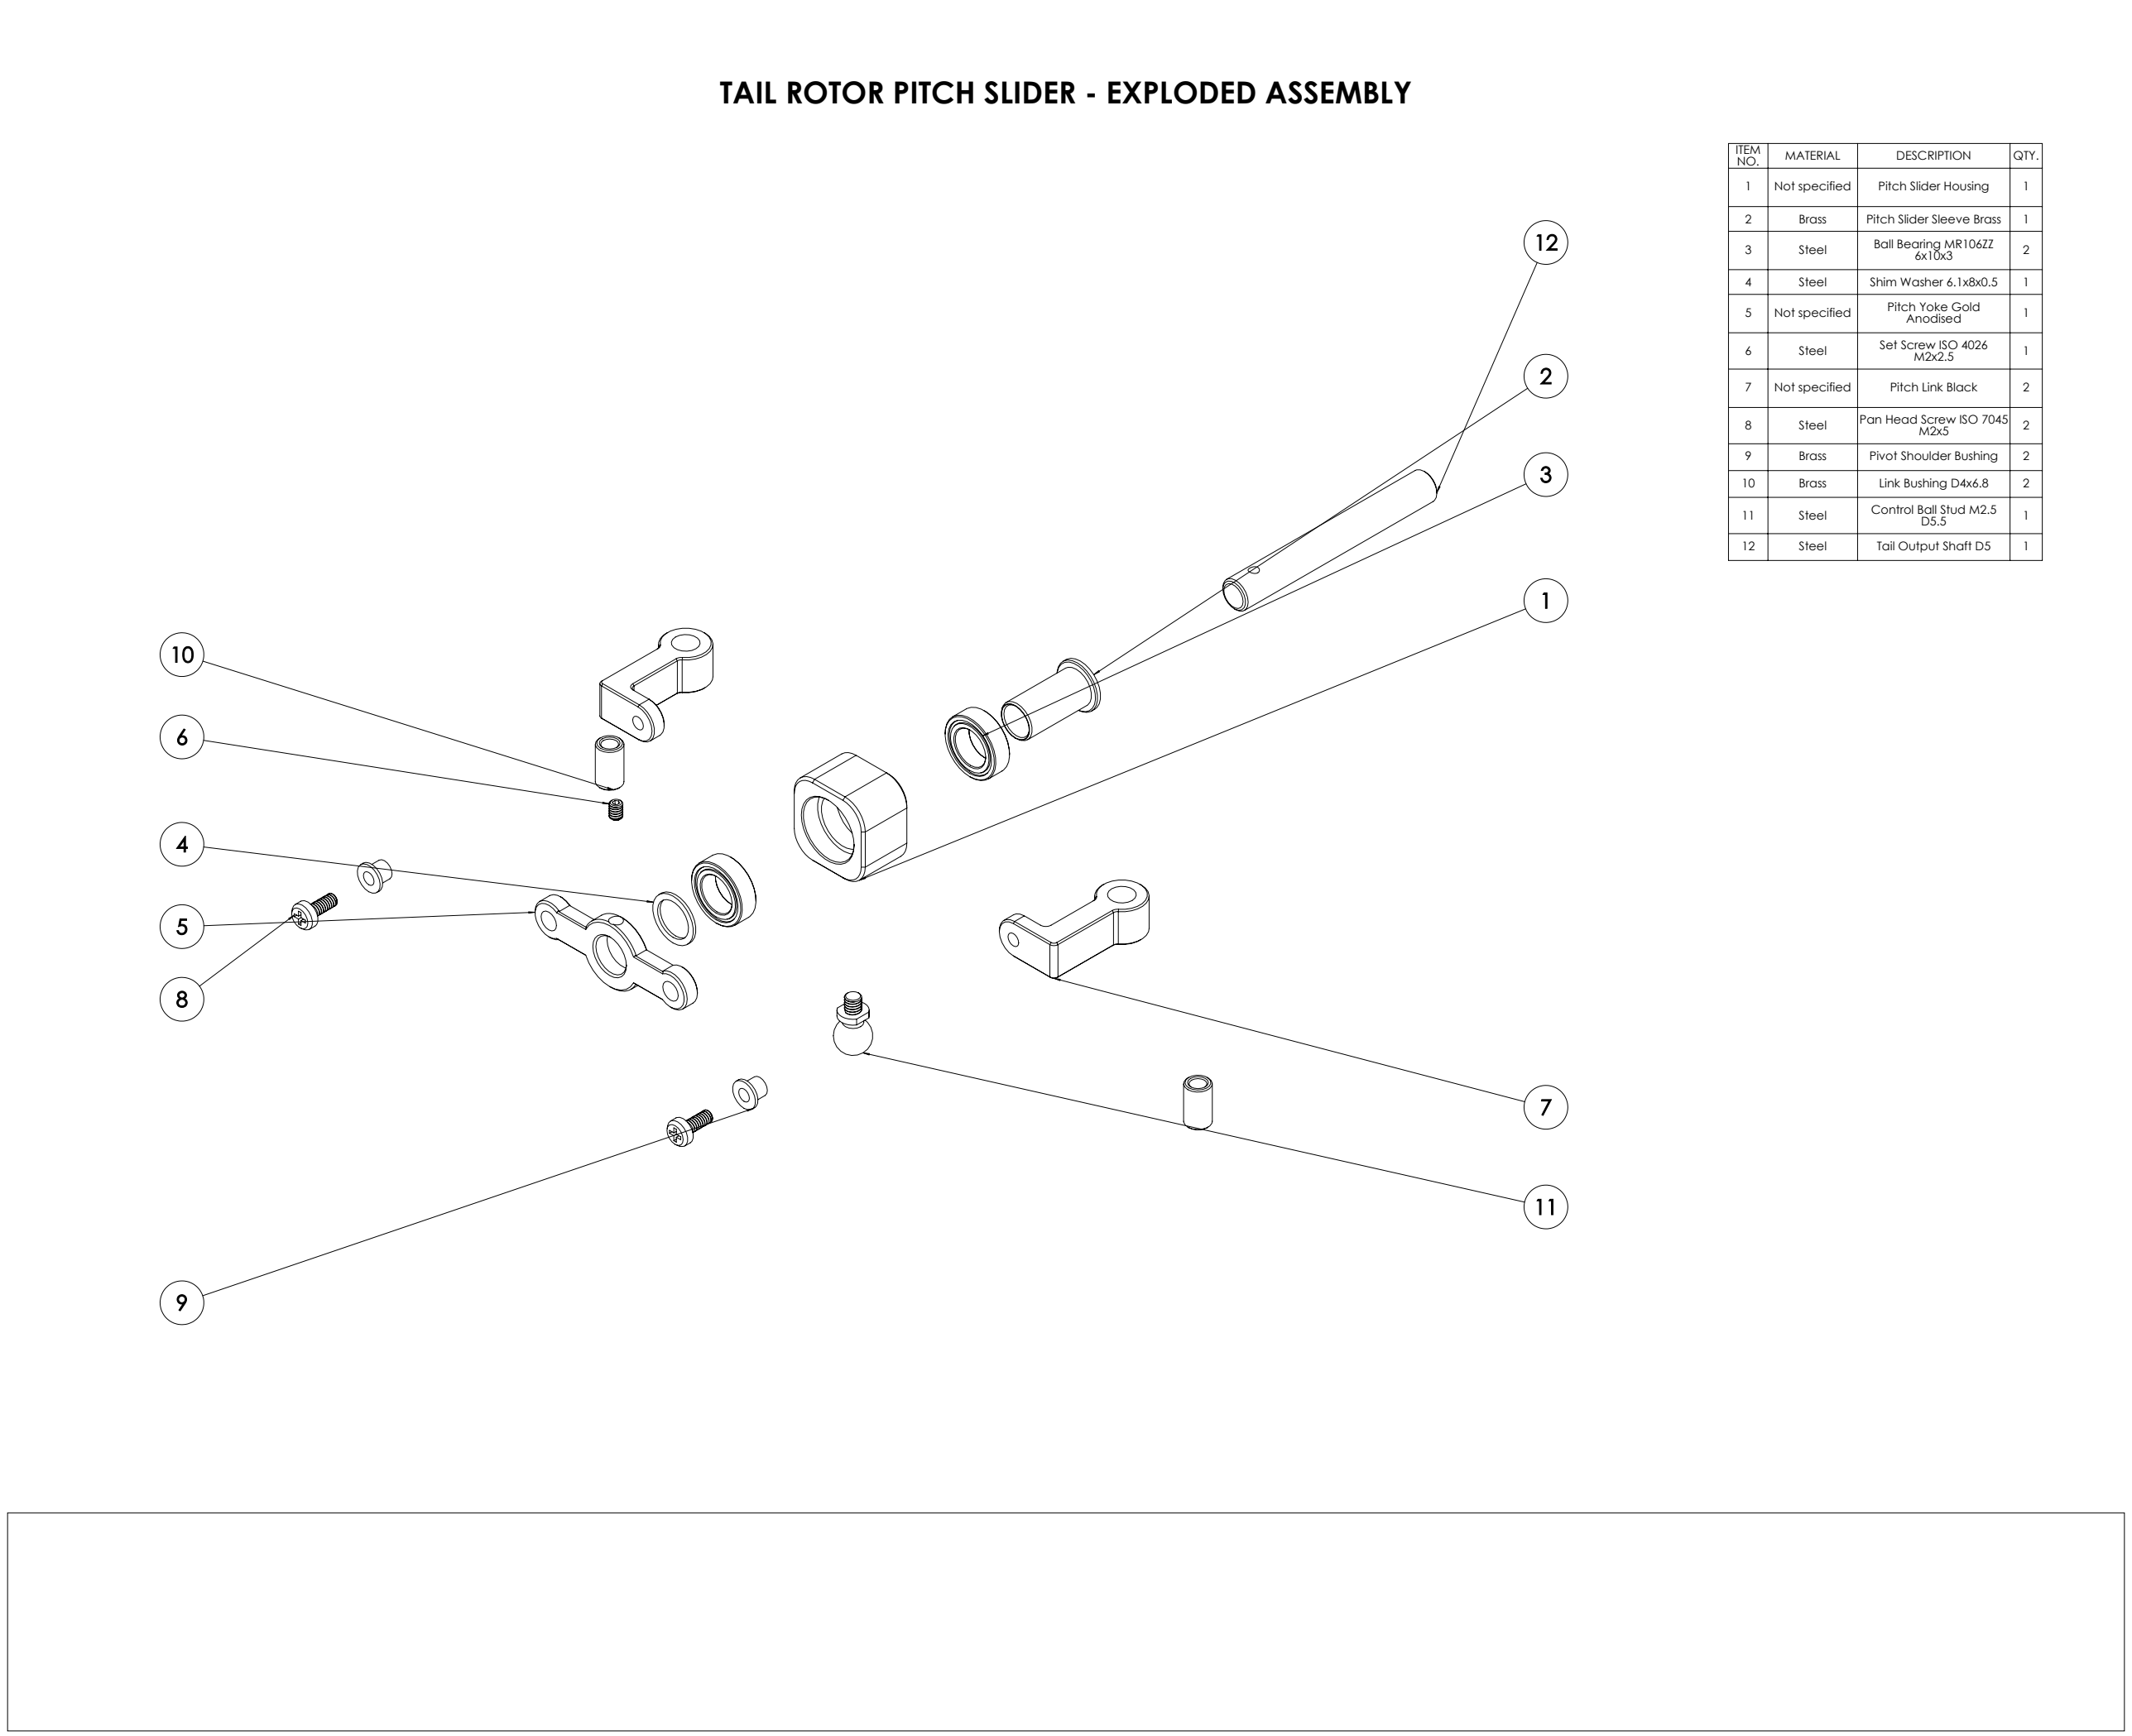
ISO-10303-21;
HEADER;
/* Generated by software containing ST-Developer
 * from STEP Tools, Inc. (www.steptools.com) 
 */

FILE_DESCRIPTION(
/* description */ (''),
/* implementation_level */ '2;1');

FILE_NAME(
/* name */ 'MAS-501',
/* time_stamp */ '2026-10-25T01:35:35-07:00',
/* author */ (''),
/* organization */ (''),
/* preprocessor_version */ 'ST-DEVELOPER v20.2',
/* originating_system */ 'Autodesk Translation Framework v15.15.0.0',
/* authorisation */ '');

FILE_SCHEMA (('AUTOMOTIVE_DESIGN { 1 0 10303 214 3 1 1 }'));
ENDSEC;

DATA;
#10=MECHANICAL_DESIGN_GEOMETRIC_PRESENTATION_REPRESENTATION('',(#260,#261,
#262,#263,#264,#265,#266,#267,#268,#269,#270,#271),#11430);
#11=ITEM_DEFINED_TRANSFORMATION($,$,#4607,#5066);
#12=ITEM_DEFINED_TRANSFORMATION($,$,#4677,#5067);
#13=ITEM_DEFINED_TRANSFORMATION($,$,#4700,#5068);
#14=ITEM_DEFINED_TRANSFORMATION($,$,#4700,#5069);
#15=ITEM_DEFINED_TRANSFORMATION($,$,#4733,#5070);
#16=ITEM_DEFINED_TRANSFORMATION($,$,#4742,#5071);
#17=ITEM_DEFINED_TRANSFORMATION($,$,#4806,#5072);
#18=ITEM_DEFINED_TRANSFORMATION($,$,#4843,#5073);
#19=ITEM_DEFINED_TRANSFORMATION($,$,#4897,#5074);
#20=ITEM_DEFINED_TRANSFORMATION($,$,#4914,#5075);
#21=ITEM_DEFINED_TRANSFORMATION($,$,#4977,#5076);
#22=ITEM_DEFINED_TRANSFORMATION($,$,#4990,#5077);
#23=ITEM_DEFINED_TRANSFORMATION($,$,#5047,#5078);
#24=ITEM_DEFINED_TRANSFORMATION($,$,#4914,#5079);
#25=ITEM_DEFINED_TRANSFORMATION($,$,#4977,#5080);
#26=ITEM_DEFINED_TRANSFORMATION($,$,#4990,#5081);
#27=ITEM_DEFINED_TRANSFORMATION($,$,#5047,#5082);
#28=(
REPRESENTATION_RELATIONSHIP($,$,#11479,#11478)
REPRESENTATION_RELATIONSHIP_WITH_TRANSFORMATION(#11)
SHAPE_REPRESENTATION_RELATIONSHIP()
);
#29=(
REPRESENTATION_RELATIONSHIP($,$,#11480,#11478)
REPRESENTATION_RELATIONSHIP_WITH_TRANSFORMATION(#12)
SHAPE_REPRESENTATION_RELATIONSHIP()
);
#30=(
REPRESENTATION_RELATIONSHIP($,$,#11481,#11478)
REPRESENTATION_RELATIONSHIP_WITH_TRANSFORMATION(#13)
SHAPE_REPRESENTATION_RELATIONSHIP()
);
#31=(
REPRESENTATION_RELATIONSHIP($,$,#11481,#11478)
REPRESENTATION_RELATIONSHIP_WITH_TRANSFORMATION(#14)
SHAPE_REPRESENTATION_RELATIONSHIP()
);
#32=(
REPRESENTATION_RELATIONSHIP($,$,#11482,#11478)
REPRESENTATION_RELATIONSHIP_WITH_TRANSFORMATION(#15)
SHAPE_REPRESENTATION_RELATIONSHIP()
);
#33=(
REPRESENTATION_RELATIONSHIP($,$,#11483,#11478)
REPRESENTATION_RELATIONSHIP_WITH_TRANSFORMATION(#16)
SHAPE_REPRESENTATION_RELATIONSHIP()
);
#34=(
REPRESENTATION_RELATIONSHIP($,$,#11484,#11478)
REPRESENTATION_RELATIONSHIP_WITH_TRANSFORMATION(#17)
SHAPE_REPRESENTATION_RELATIONSHIP()
);
#35=(
REPRESENTATION_RELATIONSHIP($,$,#11485,#11478)
REPRESENTATION_RELATIONSHIP_WITH_TRANSFORMATION(#18)
SHAPE_REPRESENTATION_RELATIONSHIP()
);
#36=(
REPRESENTATION_RELATIONSHIP($,$,#11486,#11478)
REPRESENTATION_RELATIONSHIP_WITH_TRANSFORMATION(#19)
SHAPE_REPRESENTATION_RELATIONSHIP()
);
#37=(
REPRESENTATION_RELATIONSHIP($,$,#11487,#11478)
REPRESENTATION_RELATIONSHIP_WITH_TRANSFORMATION(#20)
SHAPE_REPRESENTATION_RELATIONSHIP()
);
#38=(
REPRESENTATION_RELATIONSHIP($,$,#11488,#11478)
REPRESENTATION_RELATIONSHIP_WITH_TRANSFORMATION(#21)
SHAPE_REPRESENTATION_RELATIONSHIP()
);
#39=(
REPRESENTATION_RELATIONSHIP($,$,#11489,#11478)
REPRESENTATION_RELATIONSHIP_WITH_TRANSFORMATION(#22)
SHAPE_REPRESENTATION_RELATIONSHIP()
);
#40=(
REPRESENTATION_RELATIONSHIP($,$,#11490,#11478)
REPRESENTATION_RELATIONSHIP_WITH_TRANSFORMATION(#23)
SHAPE_REPRESENTATION_RELATIONSHIP()
);
#41=(
REPRESENTATION_RELATIONSHIP($,$,#11487,#11478)
REPRESENTATION_RELATIONSHIP_WITH_TRANSFORMATION(#24)
SHAPE_REPRESENTATION_RELATIONSHIP()
);
#42=(
REPRESENTATION_RELATIONSHIP($,$,#11488,#11478)
REPRESENTATION_RELATIONSHIP_WITH_TRANSFORMATION(#25)
SHAPE_REPRESENTATION_RELATIONSHIP()
);
#43=(
REPRESENTATION_RELATIONSHIP($,$,#11489,#11478)
REPRESENTATION_RELATIONSHIP_WITH_TRANSFORMATION(#26)
SHAPE_REPRESENTATION_RELATIONSHIP()
);
#44=(
REPRESENTATION_RELATIONSHIP($,$,#11490,#11478)
REPRESENTATION_RELATIONSHIP_WITH_TRANSFORMATION(#27)
SHAPE_REPRESENTATION_RELATIONSHIP()
);
#45=CONTEXT_DEPENDENT_SHAPE_REPRESENTATION(#28,#11461);
#46=CONTEXT_DEPENDENT_SHAPE_REPRESENTATION(#29,#11462);
#47=CONTEXT_DEPENDENT_SHAPE_REPRESENTATION(#30,#11463);
#48=CONTEXT_DEPENDENT_SHAPE_REPRESENTATION(#31,#11464);
#49=CONTEXT_DEPENDENT_SHAPE_REPRESENTATION(#32,#11465);
#50=CONTEXT_DEPENDENT_SHAPE_REPRESENTATION(#33,#11466);
#51=CONTEXT_DEPENDENT_SHAPE_REPRESENTATION(#34,#11467);
#52=CONTEXT_DEPENDENT_SHAPE_REPRESENTATION(#35,#11468);
#53=CONTEXT_DEPENDENT_SHAPE_REPRESENTATION(#36,#11469);
#54=CONTEXT_DEPENDENT_SHAPE_REPRESENTATION(#37,#11470);
#55=CONTEXT_DEPENDENT_SHAPE_REPRESENTATION(#38,#11471);
#56=CONTEXT_DEPENDENT_SHAPE_REPRESENTATION(#39,#11472);
#57=CONTEXT_DEPENDENT_SHAPE_REPRESENTATION(#40,#11473);
#58=CONTEXT_DEPENDENT_SHAPE_REPRESENTATION(#41,#11474);
#59=CONTEXT_DEPENDENT_SHAPE_REPRESENTATION(#42,#11475);
#60=CONTEXT_DEPENDENT_SHAPE_REPRESENTATION(#43,#11476);
#61=CONTEXT_DEPENDENT_SHAPE_REPRESENTATION(#44,#11477);
#62=NEXT_ASSEMBLY_USAGE_OCCURRENCE('01_Pitch_Slider_Housing:2',
'01_Pitch_Slider_Housing:2','01_Pitch_Slider_Housing:2',#11492,#11493,
'01_Pitch_Slider_Housing:2');
#63=NEXT_ASSEMBLY_USAGE_OCCURRENCE('02_Pitch_Slider_Sleeve_Brass:2',
'02_Pitch_Slider_Sleeve_Brass:2','02_Pitch_Slider_Sleeve_Brass:2',#11492,
#11494,'02_Pitch_Slider_Sleeve_Brass:2');
#64=NEXT_ASSEMBLY_USAGE_OCCURRENCE('03_Ball_Bearing_MR106ZZ_6x10x3:2',
'03_Ball_Bearing_MR106ZZ_6x10x3:2','03_Ball_Bearing_MR106ZZ_6x10x3:2',#11492,
#11495,'03_Ball_Bearing_MR106ZZ_6x10x3:2');
#65=NEXT_ASSEMBLY_USAGE_OCCURRENCE('03_Ball_Bearing_MR106ZZ_6x10x3:3',
'03_Ball_Bearing_MR106ZZ_6x10x3:3','03_Ball_Bearing_MR106ZZ_6x10x3:3',#11492,
#11495,'03_Ball_Bearing_MR106ZZ_6x10x3:3');
#66=NEXT_ASSEMBLY_USAGE_OCCURRENCE('04_Shim_Washer_6.1x8x0.5:2',
'04_Shim_Washer_6.1x8x0.5:2','04_Shim_Washer_6.1x8x0.5:2',#11492,#11496,
'04_Shim_Washer_6.1x8x0.5:2');
#67=NEXT_ASSEMBLY_USAGE_OCCURRENCE('05_Pitch_Yoke_Gold_Anodised:2',
'05_Pitch_Yoke_Gold_Anodised:2','05_Pitch_Yoke_Gold_Anodised:2',#11492,
#11497,'05_Pitch_Yoke_Gold_Anodised:2');
#68=NEXT_ASSEMBLY_USAGE_OCCURRENCE('06_Set_Screw_ISO_4026_M2x2.5:2',
'06_Set_Screw_ISO_4026_M2x2.5:2','06_Set_Screw_ISO_4026_M2x2.5:2',#11492,
#11498,'06_Set_Screw_ISO_4026_M2x2.5:2');
#69=NEXT_ASSEMBLY_USAGE_OCCURRENCE('11_Control_Ball_Stud_M2.5_D5.5:2',
'11_Control_Ball_Stud_M2.5_D5.5:2','11_Control_Ball_Stud_M2.5_D5.5:2',#11492,
#11499,'11_Control_Ball_Stud_M2.5_D5.5:2');
#70=NEXT_ASSEMBLY_USAGE_OCCURRENCE('12_Tail_Output_Shaft_D5:2',
'12_Tail_Output_Shaft_D5:2','12_Tail_Output_Shaft_D5:2',#11492,#11500,
'12_Tail_Output_Shaft_D5:2');
#71=NEXT_ASSEMBLY_USAGE_OCCURRENCE('07_Pitch_Link_Black:2',
'07_Pitch_Link_Black:2','07_Pitch_Link_Black:2',#11492,#11501,
'07_Pitch_Link_Black:2');
#72=NEXT_ASSEMBLY_USAGE_OCCURRENCE('09_Pivot_Shoulder_Bushing:2',
'09_Pivot_Shoulder_Bushing:2','09_Pivot_Shoulder_Bushing:2',#11492,#11502,
'09_Pivot_Shoulder_Bushing:2');
#73=NEXT_ASSEMBLY_USAGE_OCCURRENCE('08_Pan_Head_Screw_ISO_7045_M2x5:2',
'08_Pan_Head_Screw_ISO_7045_M2x5:2','08_Pan_Head_Screw_ISO_7045_M2x5:2',
#11492,#11503,'08_Pan_Head_Screw_ISO_7045_M2x5:2');
#74=NEXT_ASSEMBLY_USAGE_OCCURRENCE('10_Link_Bushing_D4x6.8:2',
'10_Link_Bushing_D4x6.8:2','10_Link_Bushing_D4x6.8:2',#11492,#11504,
'10_Link_Bushing_D4x6.8:2');
#75=NEXT_ASSEMBLY_USAGE_OCCURRENCE('07_Pitch_Link_Black:3',
'07_Pitch_Link_Black:3','07_Pitch_Link_Black:3',#11492,#11501,
'07_Pitch_Link_Black:3');
#76=NEXT_ASSEMBLY_USAGE_OCCURRENCE('09_Pivot_Shoulder_Bushing:3',
'09_Pivot_Shoulder_Bushing:3','09_Pivot_Shoulder_Bushing:3',#11492,#11502,
'09_Pivot_Shoulder_Bushing:3');
#77=NEXT_ASSEMBLY_USAGE_OCCURRENCE('08_Pan_Head_Screw_ISO_7045_M2x5:3',
'08_Pan_Head_Screw_ISO_7045_M2x5:3','08_Pan_Head_Screw_ISO_7045_M2x5:3',
#11492,#11503,'08_Pan_Head_Screw_ISO_7045_M2x5:3');
#78=NEXT_ASSEMBLY_USAGE_OCCURRENCE('10_Link_Bushing_D4x6.8:3',
'10_Link_Bushing_D4x6.8:3','10_Link_Bushing_D4x6.8:3',#11492,#11504,
'10_Link_Bushing_D4x6.8:3');
#79=SPHERICAL_SURFACE('',#4882,2.75);
#80=B_SPLINE_SURFACE_WITH_KNOTS('',3,3,((#7470,#7471,#7472,#7473,#7474,
#7475,#7476,#7477,#7478,#7479,#7480,#7481,#7482,#7483,#7484,#7485,#7486,
#7487,#7488,#7489,#7490,#7491,#7492,#7493,#7494,#7495,#7496,#7497,#7498,
#7499,#7500,#7501,#7502,#7503,#7504,#7505,#7506,#7507,#7508),(#7509,#7510,
#7511,#7512,#7513,#7514,#7515,#7516,#7517,#7518,#7519,#7520,#7521,#7522,
#7523,#7524,#7525,#7526,#7527,#7528,#7529,#7530,#7531,#7532,#7533,#7534,
#7535,#7536,#7537,#7538,#7539,#7540,#7541,#7542,#7543,#7544,#7545,#7546,
#7547),(#7548,#7549,#7550,#7551,#7552,#7553,#7554,#7555,#7556,#7557,#7558,
#7559,#7560,#7561,#7562,#7563,#7564,#7565,#7566,#7567,#7568,#7569,#7570,
#7571,#7572,#7573,#7574,#7575,#7576,#7577,#7578,#7579,#7580,#7581,#7582,
#7583,#7584,#7585,#7586),(#7587,#7588,#7589,#7590,#7591,#7592,#7593,#7594,
#7595,#7596,#7597,#7598,#7599,#7600,#7601,#7602,#7603,#7604,#7605,#7606,
#7607,#7608,#7609,#7610,#7611,#7612,#7613,#7614,#7615,#7616,#7617,#7618,
#7619,#7620,#7621,#7622,#7623,#7624,#7625)),.UNSPECIFIED.,.F.,.F.,.F.,(4,
4),(4,1,1,1,1,1,1,1,1,1,1,1,1,1,1,1,1,1,1,1,1,1,1,1,1,1,1,1,1,1,1,1,1,1,
1,1,4),(0.,0.0262983047615875),(8.30929135176533,9.30907769871814,10.308864045671,
11.3086503926238,12.3084367395766,13.3082230865294,14.3080094334822,15.307795780435,
16.3075821273878,17.3073684743406,18.3071548212935,19.3069411682463,20.3067275151991,
21.3065138621519,22.3063002091047,23.3060865560575,24.3058729030103,25.3056592499631,
26.305445596916,27.3052319438688,28.3050182908216,29.3048046377744,30.3045909847272,
31.30437733168,32.3041636786328,33.3039500255856,34.3037363725385,35.3035227194913,
36.3033090664441,37.3030954133969,38.3028817603497,39.3026681073025,40.3024544542553,
41.3022408012082,42.302027148161,43.3018134951138,44.3015998420666),
 .UNSPECIFIED.);
#81=B_SPLINE_SURFACE_WITH_KNOTS('',3,3,((#7807,#7808,#7809,#7810,#7811,
#7812,#7813,#7814,#7815,#7816,#7817,#7818,#7819,#7820,#7821,#7822,#7823,
#7824,#7825,#7826,#7827,#7828,#7829,#7830,#7831,#7832,#7833,#7834,#7835,
#7836,#7837,#7838,#7839,#7840,#7841,#7842,#7843,#7844,#7845),(#7846,#7847,
#7848,#7849,#7850,#7851,#7852,#7853,#7854,#7855,#7856,#7857,#7858,#7859,
#7860,#7861,#7862,#7863,#7864,#7865,#7866,#7867,#7868,#7869,#7870,#7871,
#7872,#7873,#7874,#7875,#7876,#7877,#7878,#7879,#7880,#7881,#7882,#7883,
#7884),(#7885,#7886,#7887,#7888,#7889,#7890,#7891,#7892,#7893,#7894,#7895,
#7896,#7897,#7898,#7899,#7900,#7901,#7902,#7903,#7904,#7905,#7906,#7907,
#7908,#7909,#7910,#7911,#7912,#7913,#7914,#7915,#7916,#7917,#7918,#7919,
#7920,#7921,#7922,#7923),(#7924,#7925,#7926,#7927,#7928,#7929,#7930,#7931,
#7932,#7933,#7934,#7935,#7936,#7937,#7938,#7939,#7940,#7941,#7942,#7943,
#7944,#7945,#7946,#7947,#7948,#7949,#7950,#7951,#7952,#7953,#7954,#7955,
#7956,#7957,#7958,#7959,#7960,#7961,#7962)),.UNSPECIFIED.,.F.,.F.,.F.,(4,
4),(4,1,1,1,1,1,1,1,1,1,1,1,1,1,1,1,1,1,1,1,1,1,1,1,1,1,1,1,1,1,1,1,1,1,
1,1,4),(0.,0.0262983047615875),(11.6163931973415,12.6161795442943,13.6159658912471,
14.6157522381999,15.6155385851527,16.6153249321056,17.6151112790584,18.6148976260112,
19.614683972964,20.6144703199168,21.6142566668696,22.6140430138224,23.6138293607753,
24.6136157077281,25.6134020546809,26.6131884016337,27.6129747485865,28.6127610955393,
29.6125474424921,30.6123337894449,31.6121201363978,32.6119064833506,33.6116928303034,
34.6114791772562,35.611265524209,36.6110518711618,37.6108382181146,38.6106245650675,
39.6104109120203,40.6101972589731,41.6099836059259,42.6097699528787,43.6095562998315,
44.6093426467843,45.6091289937371,46.60891534069,47.6087016876428),
 .UNSPECIFIED.);
#82=B_SPLINE_SURFACE_WITH_KNOTS('',3,3,((#8355,#8356,#8357,#8358,#8359,
#8360,#8361,#8362,#8363,#8364,#8365,#8366,#8367,#8368,#8369,#8370,#8371,
#8372,#8373,#8374,#8375,#8376,#8377,#8378,#8379,#8380,#8381,#8382,#8383,
#8384,#8385,#8386,#8387,#8388,#8389,#8390,#8391),(#8392,#8393,#8394,#8395,
#8396,#8397,#8398,#8399,#8400,#8401,#8402,#8403,#8404,#8405,#8406,#8407,
#8408,#8409,#8410,#8411,#8412,#8413,#8414,#8415,#8416,#8417,#8418,#8419,
#8420,#8421,#8422,#8423,#8424,#8425,#8426,#8427,#8428),(#8429,#8430,#8431,
#8432,#8433,#8434,#8435,#8436,#8437,#8438,#8439,#8440,#8441,#8442,#8443,
#8444,#8445,#8446,#8447,#8448,#8449,#8450,#8451,#8452,#8453,#8454,#8455,
#8456,#8457,#8458,#8459,#8460,#8461,#8462,#8463,#8464,#8465),(#8466,#8467,
#8468,#8469,#8470,#8471,#8472,#8473,#8474,#8475,#8476,#8477,#8478,#8479,
#8480,#8481,#8482,#8483,#8484,#8485,#8486,#8487,#8488,#8489,#8490,#8491,
#8492,#8493,#8494,#8495,#8496,#8497,#8498,#8499,#8500,#8501,#8502)),
 .UNSPECIFIED.,.F.,.F.,.F.,(4,4),(4,1,1,1,1,1,1,1,1,1,1,1,1,1,1,1,1,1,1,
1,1,1,1,1,1,1,1,1,1,1,1,1,1,1,4),(0.,0.0296469363228873),(8.30626835282493,
9.28498110675177,10.2636938606786,11.2424066146055,12.2211193685323,13.1998321224591,
14.178544876386,15.1572576303128,16.1359703842396,17.1146831381665,18.0933958920933,
19.0721086460202,20.050821399947,21.0295341538738,22.0082469078007,22.9869596617275,
23.9656724156544,24.9443851695812,25.923097923508,26.9018106774349,27.8805234313617,
28.8592361852886,29.8379489392154,30.8166616931422,31.7953744470691,32.7740872009959,
33.7527999549228,34.7315127088496,35.7102254627764,36.6889382167033,37.6676509706301,
38.646363724557,39.6250764784838,40.6037892324106,41.5825019863375),
 .UNSPECIFIED.);
#83=B_SPLINE_SURFACE_WITH_KNOTS('',3,3,((#8785,#8786,#8787,#8788,#8789,
#8790,#8791,#8792,#8793,#8794,#8795,#8796,#8797,#8798,#8799,#8800,#8801,
#8802,#8803,#8804,#8805,#8806,#8807,#8808,#8809,#8810,#8811,#8812,#8813,
#8814,#8815,#8816,#8817,#8818,#8819,#8820,#8821),(#8822,#8823,#8824,#8825,
#8826,#8827,#8828,#8829,#8830,#8831,#8832,#8833,#8834,#8835,#8836,#8837,
#8838,#8839,#8840,#8841,#8842,#8843,#8844,#8845,#8846,#8847,#8848,#8849,
#8850,#8851,#8852,#8853,#8854,#8855,#8856,#8857,#8858),(#8859,#8860,#8861,
#8862,#8863,#8864,#8865,#8866,#8867,#8868,#8869,#8870,#8871,#8872,#8873,
#8874,#8875,#8876,#8877,#8878,#8879,#8880,#8881,#8882,#8883,#8884,#8885,
#8886,#8887,#8888,#8889,#8890,#8891,#8892,#8893,#8894,#8895),(#8896,#8897,
#8898,#8899,#8900,#8901,#8902,#8903,#8904,#8905,#8906,#8907,#8908,#8909,
#8910,#8911,#8912,#8913,#8914,#8915,#8916,#8917,#8918,#8919,#8920,#8921,
#8922,#8923,#8924,#8925,#8926,#8927,#8928,#8929,#8930,#8931,#8932)),
 .UNSPECIFIED.,.F.,.F.,.F.,(4,4),(4,1,1,1,1,1,1,1,1,1,1,1,1,1,1,1,1,1,1,
1,1,1,1,1,1,1,1,1,1,1,1,1,1,1,4),(0.,0.0296469363228873),(11.6151336144497,
12.5938463683765,13.5725591223033,14.5512718762302,15.529984630157,16.5086973840839,
17.4874101380107,18.4661228919375,19.4448356458644,20.4235483997912,21.4022611537181,
22.3809739076449,23.3596866615717,24.3383994154986,25.3171121694254,26.2958249233523,
27.2745376772791,28.2532504312059,29.2319631851328,30.2106759390596,31.1893886929865,
32.1681014469133,33.1468142008401,34.125526954767,35.1042397086938,36.0829524626207,
37.0616652165475,38.0403779704743,39.0190907244012,39.997803478328,40.9765162322549,
41.9552289861817,42.9339417401085,43.9126544940354,44.8913672479622),
 .UNSPECIFIED.);
#84=B_SPLINE_SURFACE_WITH_KNOTS('',3,3,((#10251,#10252,#10253,#10254,#10255,
#10256,#10257,#10258,#10259,#10260,#10261,#10262,#10263,#10264,#10265,#10266,
#10267,#10268,#10269,#10270,#10271,#10272,#10273,#10274,#10275,#10276,#10277,
#10278,#10279,#10280,#10281,#10282,#10283,#10284,#10285,#10286,#10287,#10288,
#10289,#10290,#10291,#10292,#10293,#10294,#10295,#10296,#10297,#10298,#10299,
#10300,#10301,#10302,#10303,#10304,#10305,#10306,#10307,#10308,#10309,#10310,
#10311,#10312,#10313,#10314,#10315,#10316,#10317,#10318,#10319,#10320,#10321,
#10322,#10323,#10324,#10325,#10326,#10327,#10328,#10329,#10330,#10331),
(#10332,#10333,#10334,#10335,#10336,#10337,#10338,#10339,#10340,#10341,
#10342,#10343,#10344,#10345,#10346,#10347,#10348,#10349,#10350,#10351,#10352,
#10353,#10354,#10355,#10356,#10357,#10358,#10359,#10360,#10361,#10362,#10363,
#10364,#10365,#10366,#10367,#10368,#10369,#10370,#10371,#10372,#10373,#10374,
#10375,#10376,#10377,#10378,#10379,#10380,#10381,#10382,#10383,#10384,#10385,
#10386,#10387,#10388,#10389,#10390,#10391,#10392,#10393,#10394,#10395,#10396,
#10397,#10398,#10399,#10400,#10401,#10402,#10403,#10404,#10405,#10406,#10407,
#10408,#10409,#10410,#10411,#10412),(#10413,#10414,#10415,#10416,#10417,
#10418,#10419,#10420,#10421,#10422,#10423,#10424,#10425,#10426,#10427,#10428,
#10429,#10430,#10431,#10432,#10433,#10434,#10435,#10436,#10437,#10438,#10439,
#10440,#10441,#10442,#10443,#10444,#10445,#10446,#10447,#10448,#10449,#10450,
#10451,#10452,#10453,#10454,#10455,#10456,#10457,#10458,#10459,#10460,#10461,
#10462,#10463,#10464,#10465,#10466,#10467,#10468,#10469,#10470,#10471,#10472,
#10473,#10474,#10475,#10476,#10477,#10478,#10479,#10480,#10481,#10482,#10483,
#10484,#10485,#10486,#10487,#10488,#10489,#10490,#10491,#10492,#10493),
(#10494,#10495,#10496,#10497,#10498,#10499,#10500,#10501,#10502,#10503,
#10504,#10505,#10506,#10507,#10508,#10509,#10510,#10511,#10512,#10513,#10514,
#10515,#10516,#10517,#10518,#10519,#10520,#10521,#10522,#10523,#10524,#10525,
#10526,#10527,#10528,#10529,#10530,#10531,#10532,#10533,#10534,#10535,#10536,
#10537,#10538,#10539,#10540,#10541,#10542,#10543,#10544,#10545,#10546,#10547,
#10548,#10549,#10550,#10551,#10552,#10553,#10554,#10555,#10556,#10557,#10558,
#10559,#10560,#10561,#10562,#10563,#10564,#10565,#10566,#10567,#10568,#10569,
#10570,#10571,#10572,#10573,#10574)),.UNSPECIFIED.,.F.,.F.,.F.,(4,4),(4,
1,1,1,1,1,1,1,1,1,1,1,1,1,1,1,1,1,1,1,1,1,1,1,1,1,1,1,1,1,1,1,1,1,1,1,1,
1,1,1,1,1,1,1,1,1,1,1,1,1,1,1,1,1,1,1,1,1,1,1,1,1,1,1,1,1,1,1,1,1,1,1,1,
1,1,1,1,1,4),(0.,0.0262983047615875),(8.30929135176529,9.30911157600678,
10.3089318002483,11.3087520244898,12.3085722487312,13.3083924729727,14.3082126972142,
15.3080329214557,16.3078531456972,17.3076733699387,18.3074935941802,19.3073138184217,
20.3071340426631,21.3069542669046,22.3067744911461,23.3065947153876,24.3064149396291,
25.3062351638706,26.3060553881121,27.3058756123536,28.305695836595,29.3055160608365,
30.305336285078,31.3051565093195,32.304976733561,33.3047969578025,34.304617182044,
35.3044374062855,36.3042576305269,37.3040778547684,38.3038980790099,39.3037183032514,
40.3035385274929,41.3033587517344,42.3031789759759,43.3029992002174,44.3028194244588,
45.3026396487003,46.3024598729418,47.3022800971833,48.3021003214248,49.3019205456663,
50.3017407699078,51.3015609941492,52.3013812183907,53.3012014426322,54.3010216668737,
55.3008418911152,56.3006621153567,57.3004823395982,58.3003025638397,59.3001227880811,
60.2999430123226,61.2997632365641,62.2995834608056,63.2994036850471,64.2992239092886,
65.2990441335301,66.2988643577716,67.298684582013,68.2985048062545,69.298325030496,
70.2981452547375,71.297965478979,72.2977857032205,73.297605927462,74.2974261517035,
75.297246375945,76.2970666001864,77.2968868244279,78.2967070486694,79.2965272729109,
80.2963474971524,81.2961677213939,82.2959879456354,83.2958081698768,84.2956283941183,
85.2954486183598,86.2952688426013),.UNSPECIFIED.);
#85=B_SPLINE_SURFACE_WITH_KNOTS('',3,3,((#10842,#10843,#10844,#10845,#10846,
#10847,#10848,#10849,#10850,#10851,#10852,#10853,#10854,#10855,#10856,#10857,
#10858,#10859,#10860,#10861,#10862,#10863,#10864,#10865,#10866,#10867,#10868,
#10869,#10870,#10871,#10872,#10873,#10874,#10875,#10876,#10877,#10878,#10879,
#10880,#10881,#10882,#10883,#10884,#10885,#10886,#10887,#10888,#10889,#10890,
#10891,#10892,#10893,#10894,#10895,#10896,#10897,#10898,#10899,#10900,#10901,
#10902,#10903,#10904,#10905,#10906,#10907,#10908,#10909,#10910,#10911,#10912,
#10913,#10914,#10915,#10916,#10917,#10918,#10919,#10920,#10921,#10922),
(#10923,#10924,#10925,#10926,#10927,#10928,#10929,#10930,#10931,#10932,
#10933,#10934,#10935,#10936,#10937,#10938,#10939,#10940,#10941,#10942,#10943,
#10944,#10945,#10946,#10947,#10948,#10949,#10950,#10951,#10952,#10953,#10954,
#10955,#10956,#10957,#10958,#10959,#10960,#10961,#10962,#10963,#10964,#10965,
#10966,#10967,#10968,#10969,#10970,#10971,#10972,#10973,#10974,#10975,#10976,
#10977,#10978,#10979,#10980,#10981,#10982,#10983,#10984,#10985,#10986,#10987,
#10988,#10989,#10990,#10991,#10992,#10993,#10994,#10995,#10996,#10997,#10998,
#10999,#11000,#11001,#11002,#11003),(#11004,#11005,#11006,#11007,#11008,
#11009,#11010,#11011,#11012,#11013,#11014,#11015,#11016,#11017,#11018,#11019,
#11020,#11021,#11022,#11023,#11024,#11025,#11026,#11027,#11028,#11029,#11030,
#11031,#11032,#11033,#11034,#11035,#11036,#11037,#11038,#11039,#11040,#11041,
#11042,#11043,#11044,#11045,#11046,#11047,#11048,#11049,#11050,#11051,#11052,
#11053,#11054,#11055,#11056,#11057,#11058,#11059,#11060,#11061,#11062,#11063,
#11064,#11065,#11066,#11067,#11068,#11069,#11070,#11071,#11072,#11073,#11074,
#11075,#11076,#11077,#11078,#11079,#11080,#11081,#11082,#11083,#11084),
(#11085,#11086,#11087,#11088,#11089,#11090,#11091,#11092,#11093,#11094,
#11095,#11096,#11097,#11098,#11099,#11100,#11101,#11102,#11103,#11104,#11105,
#11106,#11107,#11108,#11109,#11110,#11111,#11112,#11113,#11114,#11115,#11116,
#11117,#11118,#11119,#11120,#11121,#11122,#11123,#11124,#11125,#11126,#11127,
#11128,#11129,#11130,#11131,#11132,#11133,#11134,#11135,#11136,#11137,#11138,
#11139,#11140,#11141,#11142,#11143,#11144,#11145,#11146,#11147,#11148,#11149,
#11150,#11151,#11152,#11153,#11154,#11155,#11156,#11157,#11158,#11159,#11160,
#11161,#11162,#11163,#11164,#11165)),.UNSPECIFIED.,.F.,.F.,.F.,(4,4),(4,
1,1,1,1,1,1,1,1,1,1,1,1,1,1,1,1,1,1,1,1,1,1,1,1,1,1,1,1,1,1,1,1,1,1,1,1,
1,1,1,1,1,1,1,1,1,1,1,1,1,1,1,1,1,1,1,1,1,1,1,1,1,1,1,1,1,1,1,1,1,1,1,1,
1,1,1,1,1,4),(0.,0.0262983047615875),(11.6163931973414,12.6162134215829,
13.6160336458244,14.6158538700659,15.6156740943074,16.6154943185489,17.6153145427904,
18.6151347670319,19.6149549912733,20.6147752155148,21.6145954397563,22.6144156639978,
23.6142358882393,24.6140561124808,25.6138763367223,26.6136965609638,27.6135167852052,
28.6133370094467,29.6131572336882,30.6129774579297,31.6127976821712,32.6126179064127,
33.6124381306542,34.6122583548957,35.6120785791371,36.6118988033786,37.6117190276201,
38.6115392518616,39.6113594761031,40.6111797003446,41.6109999245861,42.6108201488276,
43.610640373069,44.6104605973105,45.610280821552,46.6101010457935,47.609921270035,
48.6097414942765,49.609561718518,50.6093819427595,51.6092021670009,52.6090223912424,
53.6088426154839,54.6086628397254,55.6084830639669,56.6083032882084,57.6081235124499,
58.6079437366914,59.6077639609328,60.6075841851743,61.6074044094158,62.6072246336573,
63.6070448578988,64.6068650821403,65.6066853063818,66.6065055306233,67.6063257548647,
68.6061459791062,69.6059662033477,70.6057864275892,71.6056066518307,72.6054268760722,
73.6052471003137,74.6050673245552,75.6048875487966,76.6047077730381,77.6045279972796,
78.6043482215211,79.6041684457626,80.6039886700041,81.6038088942456,82.6036291184871,
83.6034493427286,84.60326956697,85.6030897912115,86.602910015453,87.6027302396945,
88.602550463936,89.6023706881775),.UNSPECIFIED.);
#86=B_SPLINE_CURVE_WITH_KNOTS('',3,(#6723,#6724,#6725,#6726),
 .UNSPECIFIED.,.F.,.F.,(4,4),(-0.0309968818258504,0.),.UNSPECIFIED.);
#87=B_SPLINE_CURVE_WITH_KNOTS('',3,(#6727,#6728,#6729,#6730),
 .UNSPECIFIED.,.F.,.F.,(4,4),(-0.0290771795561931,0.),.UNSPECIFIED.);
#88=B_SPLINE_CURVE_WITH_KNOTS('',3,(#6734,#6735,#6736,#6737),
 .UNSPECIFIED.,.F.,.F.,(4,4),(-0.0309968818257846,0.),.UNSPECIFIED.);
#89=B_SPLINE_CURVE_WITH_KNOTS('',3,(#6742,#6743,#6744,#6745),
 .UNSPECIFIED.,.F.,.F.,(4,4),(-0.0290773085804053,0.),.UNSPECIFIED.);
#90=B_SPLINE_CURVE_WITH_KNOTS('',3,(#6748,#6749,#6750,#6751),
 .UNSPECIFIED.,.F.,.F.,(4,4),(-0.0290771795561931,0.),.UNSPECIFIED.);
#91=B_SPLINE_CURVE_WITH_KNOTS('',3,(#6757,#6758,#6759,#6760),
 .UNSPECIFIED.,.F.,.F.,(4,4),(-0.0309968818258147,0.),.UNSPECIFIED.);
#92=B_SPLINE_CURVE_WITH_KNOTS('',3,(#6767,#6768,#6769,#6770),
 .UNSPECIFIED.,.F.,.F.,(4,4),(-0.030996881825835,0.),.UNSPECIFIED.);
#93=B_SPLINE_CURVE_WITH_KNOTS('',3,(#6774,#6775,#6776,#6777),
 .UNSPECIFIED.,.F.,.F.,(4,4),(-0.0290771795558996,0.),.UNSPECIFIED.);
#94=B_SPLINE_CURVE_WITH_KNOTS('',3,(#6787,#6788,#6789,#6790,#6791,#6792,
#6793,#6794,#6795,#6796,#6797,#6798,#6799,#6800,#6801,#6802,#6803),
 .UNSPECIFIED.,.F.,.F.,(4,2,2,2,3,2,2,4),(0.475883554626383,0.515539598201686,
0.555195641776989,0.594853523972749,0.63451140616851,0.674169288364271,
0.713827170560032,0.748840077704135),.UNSPECIFIED.);
#95=B_SPLINE_CURVE_WITH_KNOTS('',3,(#6818,#6819,#6820,#6821,#6822,#6823,
#6824,#6825,#6826,#6827),.UNSPECIFIED.,.F.,.F.,(4,2,2,2,4),(0.119476318069872,
0.130197921487587,0.164602551565189,0.199007181642792,0.209728785060507),
 .UNSPECIFIED.);
#96=B_SPLINE_CURVE_WITH_KNOTS('',3,(#6832,#6833,#6834,#6835,#6836,#6837,
#6838,#6839),.UNSPECIFIED.,.F.,.F.,(4,2,2,4),(0.20292703154863,0.237939938692733,
0.277597820888494,0.317255703084255),.UNSPECIFIED.);
#97=B_SPLINE_CURVE_WITH_KNOTS('',3,(#6840,#6841,#6842,#6843,#6844,#6845,
#6846,#6847,#6848,#6849),.UNSPECIFIED.,.F.,.F.,(4,2,2,2,4),(0.317255703084255,
0.356913585280016,0.396571467475777,0.43622751105108,0.475883554626383),
 .UNSPECIFIED.);
#98=B_SPLINE_CURVE_WITH_KNOTS('',3,(#6856,#6857,#6858,#6859,#6860,#6861,
#6862,#6863,#6864,#6865,#6866,#6867,#6868,#6869),.UNSPECIFIED.,.F.,.F.,
(4,2,2,2,2,2,4),(0.389725630667101,0.399201782687169,0.439108489087217,
0.479015195487264,0.518921901887312,0.55882860828736,0.568304760307428),
 .UNSPECIFIED.);
#99=B_SPLINE_CURVE_WITH_KNOTS('',3,(#6873,#6874,#6875,#6876,#6877,#6878),
 .UNSPECIFIED.,.F.,.F.,(4,2,4),(0.204141306797506,0.239485144629183,0.248961296649252),
 .UNSPECIFIED.);
#100=B_SPLINE_CURVE_WITH_KNOTS('',3,(#6880,#6881,#6882,#6883,#6884,#6885,
#6886,#6887,#6888,#6889),.UNSPECIFIED.,.F.,.F.,(4,2,2,2,4),(0.238592722720123,
0.259879734519813,0.28491657542964,0.309953416339467,0.331240428139157),
 .UNSPECIFIED.);
#101=B_SPLINE_CURVE_WITH_KNOTS('',3,(#6891,#6892,#6893,#6894,#6895,#6896),
 .UNSPECIFIED.,.F.,.F.,(4,2,4),(0.0703821670089247,0.079858319028993,0.115202156860671),
 .UNSPECIFIED.);
#102=B_SPLINE_CURVE_WITH_KNOTS('',3,(#6930,#6931,#6932,#6933,#6934,#6935,
#6936,#6937,#6938,#6939),.UNSPECIFIED.,.F.,.F.,(4,3,3,4),(-4.09157007060746,
-3.99914538781125,-2.99935904085844,-2.06546402602172),.UNSPECIFIED.);
#103=B_SPLINE_CURVE_WITH_KNOTS('',3,(#6942,#6943,#6944,#6945,#6946,#6947,
#6948),.UNSPECIFIED.,.F.,.F.,(4,3,4),(0.,0.999786346952812,1.11548660900404),
 .UNSPECIFIED.);
#104=B_SPLINE_CURVE_WITH_KNOTS('',3,(#6953,#6954,#6955,#6956,#6957,#6958,
#6959,#6960,#6961,#6962,#6963,#6964,#6965,#6966,#6967,#6968,#6969,#6970,
#6971,#6972,#6973,#6974),.UNSPECIFIED.,.F.,.F.,(4,3,3,3,3,3,3,4),(-10.3747553777871,
-9.99786346952814,-8.99807712257532,-7.99829077562251,-6.99850442866969,
-5.99871808171688,-4.99893173476407,-4.09157007060746),.UNSPECIFIED.);
#105=B_SPLINE_CURVE_WITH_KNOTS('',3,(#6975,#6976,#6977,#6978,#6979,#6980,
#6981,#6982,#6983,#6984,#6985,#6986,#6987,#6988,#6989,#6990,#6991,#6992,
#6993,#6994,#6995,#6996),.UNSPECIFIED.,.F.,.F.,(4,3,3,3,3,3,3,4),(1.11548660900404,
1.99957269390563,2.99935904085844,3.99914538781125,4.99893173476407,5.99871808171688,
6.99850442866969,7.39867191618363),.UNSPECIFIED.);
#106=B_SPLINE_CURVE_WITH_KNOTS('',3,(#7001,#7002,#7003,#7004,#7005,#7006,
#7007,#7008,#7009,#7010,#7011,#7012,#7013,#7014,#7015,#7016,#7017,#7018,
#7019,#7020,#7021,#7022),.UNSPECIFIED.,.F.,.F.,(4,3,3,3,3,3,3,4),(-16.6579406849666,
-15.996581551245,-14.9967952042922,-13.9970088573394,-12.9972225103866,
-11.9974361634338,-10.9976498164809,-10.3747553777871),.UNSPECIFIED.);
#107=B_SPLINE_CURVE_WITH_KNOTS('',3,(#7023,#7024,#7025,#7026,#7027,#7028,
#7029,#7030,#7031,#7032,#7033,#7034,#7035,#7036,#7037,#7038,#7039,#7040,
#7041,#7042,#7043,#7044),.UNSPECIFIED.,.F.,.F.,(4,3,3,3,3,3,3,4),(7.39867191618363,
7.99829077562251,8.99807712257532,9.99786346952813,10.9976498164809,11.9974361634338,
12.9972225103866,13.6818572233632),.UNSPECIFIED.);
#108=B_SPLINE_CURVE_WITH_KNOTS('',3,(#7049,#7050,#7051,#7052,#7053,#7054,
#7055,#7056,#7057,#7058,#7059,#7060,#7061,#7062,#7063,#7064,#7065,#7066,
#7067,#7068,#7069,#7070),.UNSPECIFIED.,.F.,.F.,(4,3,3,3,3,3,3,4),(-22.9411259921462,
-21.9952996329619,-20.9955132860091,-19.9957269390563,-18.9959405921035,
-17.9961542451506,-16.9963678981978,-16.6579406849666),.UNSPECIFIED.);
#109=B_SPLINE_CURVE_WITH_KNOTS('',3,(#7071,#7072,#7073,#7074,#7075,#7076,
#7077,#7078,#7079,#7080,#7081,#7082,#7083,#7084,#7085,#7086,#7087,#7088,
#7089,#7090,#7091,#7092),.UNSPECIFIED.,.F.,.F.,(4,3,3,3,3,3,3,4),(13.6818572233632,
13.9970088573394,14.9967952042922,15.996581551245,16.9963678981978,17.9961542451506,
18.9959405921034,19.9650425305428),.UNSPECIFIED.);
#110=B_SPLINE_CURVE_WITH_KNOTS('',3,(#7097,#7098,#7099,#7100,#7101,#7102,
#7103,#7104,#7105,#7106,#7107,#7108,#7109,#7110,#7111,#7112,#7113,#7114,
#7115,#7116,#7117,#7118,#7119,#7120,#7121),.UNSPECIFIED.,.F.,.F.,(4,3,3,
3,3,3,3,3,4),(-29.2243112993258,-28.9938040616316,-27.9940177146788,-26.994231367726,
-25.9944450207731,-24.9946586738203,-23.9948723268675,-22.9950859799147,
-22.9411259921462),.UNSPECIFIED.);
#111=B_SPLINE_CURVE_WITH_KNOTS('',3,(#7122,#7123,#7124,#7125,#7126,#7127,
#7128,#7129,#7130,#7131,#7132,#7133,#7134,#7135,#7136,#7137,#7138,#7139,
#7140,#7141,#7142,#7143,#7144,#7145,#7146),.UNSPECIFIED.,.F.,.F.,(4,3,3,
3,3,3,3,3,4),(19.9650425305428,19.9957269390563,20.9955132860091,21.9952996329619,
22.9950859799147,23.9948723268675,24.9946586738203,25.9944450207731,26.2482278377224),
 .UNSPECIFIED.);
#112=B_SPLINE_CURVE_WITH_KNOTS('',3,(#7151,#7152,#7153,#7154,#7155,#7156,
#7157,#7158,#7159,#7160,#7161,#7162,#7163,#7164,#7165,#7166,#7167,#7168,
#7169,#7170,#7171,#7172),.UNSPECIFIED.,.F.,.F.,(4,3,3,3,3,3,3,4),(-35.5074966065054,
-34.9925221433485,-33.9927357963956,-32.9929494494428,-31.99316310249,-30.9933767555372,
-29.9935904085844,-29.2243112993258),.UNSPECIFIED.);
#113=B_SPLINE_CURVE_WITH_KNOTS('',3,(#7173,#7174,#7175,#7176,#7177,#7178,
#7179,#7180,#7181,#7182,#7183,#7184,#7185,#7186,#7187,#7188,#7189,#7190,
#7191,#7192,#7193,#7194),.UNSPECIFIED.,.F.,.F.,(4,3,3,3,3,3,3,4),(26.2482278377224,
26.994231367726,27.9940177146788,28.9938040616316,29.9935904085844,30.9933767555372,
31.99316310249,32.531413144902),.UNSPECIFIED.);
#114=B_SPLINE_CURVE_WITH_KNOTS('',3,(#7200,#7201,#7202,#7203,#7204,#7205,
#7206,#7207),.UNSPECIFIED.,.F.,.F.,(4,1,1,1,1,4),(40.8407044966673,41.6099836059259,
42.6097699528787,43.6095562998315,44.6093426467843,45.5432376616211),
 .UNSPECIFIED.);
#115=B_SPLINE_CURVE_WITH_KNOTS('',3,(#7210,#7211,#7212,#7213,#7214,#7215,
#7216),.UNSPECIFIED.,.F.,.F.,(4,1,1,1,4),(40.8407044966673,41.3022408012082,
42.302027148161,43.3018134951138,44.3015998420666),.UNSPECIFIED.);
#116=B_SPLINE_CURVE_WITH_KNOTS('',3,(#7221,#7222,#7223,#7224,#7225,#7226,
#7227,#7228,#7229,#7230,#7231),.UNSPECIFIED.,.F.,.F.,(4,1,1,1,1,1,1,1,4),
(34.5575191894877,34.6114791772562,35.611265524209,36.6110518711618,37.6108382181146,
38.6106245650675,39.6104109120203,40.6101972589731,40.8407044966673),
 .UNSPECIFIED.);
#117=B_SPLINE_CURVE_WITH_KNOTS('',3,(#7232,#7233,#7234,#7235,#7236,#7237,
#7238,#7239,#7240,#7241),.UNSPECIFIED.,.F.,.F.,(4,1,1,1,1,1,1,4),(34.5575191894877,
35.3035227194913,36.3033090664441,37.3030954133969,38.3028817603497,39.3026681073025,
40.3024544542553,40.8407044966673),.UNSPECIFIED.);
#118=B_SPLINE_CURVE_WITH_KNOTS('',3,(#7246,#7247,#7248,#7249,#7250,#7251,
#7252,#7253,#7254,#7255),.UNSPECIFIED.,.F.,.F.,(4,1,1,1,1,1,1,4),(28.2743338823081,
28.6127610955393,29.6125474424921,30.6123337894449,31.6121201363978,32.6119064833506,
33.6116928303034,34.5575191894877),.UNSPECIFIED.);
#119=B_SPLINE_CURVE_WITH_KNOTS('',3,(#7256,#7257,#7258,#7259,#7260,#7261,
#7262,#7263,#7264,#7265,#7266),.UNSPECIFIED.,.F.,.F.,(4,1,1,1,1,1,1,1,4),
(28.2743338823081,28.3050182908216,29.3048046377744,30.3045909847272,31.30437733168,
32.3041636786328,33.3039500255856,34.3037363725385,34.5575191894877),
 .UNSPECIFIED.);
#120=B_SPLINE_CURVE_WITH_KNOTS('',3,(#7271,#7272,#7273,#7274,#7275,#7276,
#7277,#7278,#7279,#7280),.UNSPECIFIED.,.F.,.F.,(4,1,1,1,1,1,1,4),(21.9911485751285,
22.6140430138224,23.6138293607753,24.6136157077281,25.6134020546809,26.6131884016337,
27.6129747485865,28.2743338823081),.UNSPECIFIED.);
#121=B_SPLINE_CURVE_WITH_KNOTS('',3,(#7281,#7282,#7283,#7284,#7285,#7286,
#7287,#7288,#7289,#7290),.UNSPECIFIED.,.F.,.F.,(4,1,1,1,1,1,1,4),(21.9911485751285,
22.3063002091047,23.3060865560575,24.3058729030103,25.3056592499631,26.305445596916,
27.3052319438688,28.2743338823081),.UNSPECIFIED.);
#122=B_SPLINE_CURVE_WITH_KNOTS('',3,(#7295,#7296,#7297,#7298,#7299,#7300,
#7301,#7302,#7303,#7304),.UNSPECIFIED.,.F.,.F.,(4,1,1,1,1,1,1,4),(15.707963267949,
16.6153249321056,17.6151112790584,18.6148976260112,19.614683972964,20.6144703199168,
21.6142566668696,21.9911485751285),.UNSPECIFIED.);
#123=B_SPLINE_CURVE_WITH_KNOTS('',3,(#7305,#7306,#7307,#7308,#7309,#7310,
#7311,#7312,#7313,#7314),.UNSPECIFIED.,.F.,.F.,(4,1,1,1,1,1,1,4),(15.707963267949,
16.3075821273878,17.3073684743406,18.3071548212935,19.3069411682463,20.3067275151991,
21.3065138621519,21.9911485751285),.UNSPECIFIED.);
#124=B_SPLINE_CURVE_WITH_KNOTS('',3,(#7317,#7318,#7319,#7320,#7321,#7322,
#7323,#7324,#7325,#7326,#7327,#7328,#7329,#7330,#7331,#7332,#7333,#7334,
#7335,#7336,#7337,#7338,#7339,#7340,#7341,#7342,#7343,#7344,#7345,#7346,
#7347,#7348,#7349,#7350,#7351,#7352,#7353,#7354,#7355,#7356,#7357,#7358,
#7359,#7360,#7361,#7362,#7363,#7364,#7365,#7366,#7367,#7368,#7369,#7370,
#7371,#7372,#7373,#7374,#7375,#7376,#7377,#7378,#7379,#7380,#7381,#7382,
#7383,#7384,#7385,#7386,#7387,#7388,#7389,#7390,#7391,#7392),
 .UNSPECIFIED.,.F.,.F.,(4,3,3,3,3,3,3,3,3,3,3,3,3,3,3,3,3,3,3,3,3,3,3,3,
3,4),(-0.178587760439504,-0.17361180774909,-0.163438350924944,-0.158375688276003,
-0.155636584119497,-0.144832458277613,-0.140259732391418,-0.137183188509201,
-0.134746510299358,-0.123387595779259,-0.111954473335422,-0.106069923958762,
-0.103723902609418,-0.0922241531559208,-0.0806961340114307,-0.0752220429825342,
-0.0719210107775354,-0.0694880548095068,-0.0575218446312738,-0.045279006273988,
-0.0393960404635036,-0.0368040337146181,-0.0343328896694744,-0.0216376030695688,
-0.00903059604707899,0.),.UNSPECIFIED.);
#125=B_SPLINE_CURVE_WITH_KNOTS('',3,(#7397,#7398,#7399,#7400,#7401,#7402,
#7403,#7404,#7405,#7406,#7407,#7408,#7409,#7410,#7411,#7412,#7413,#7414,
#7415,#7416,#7417,#7418,#7419,#7420,#7421,#7422,#7423,#7424,#7425,#7426,
#7427,#7428,#7429,#7430,#7431,#7432,#7433,#7434,#7435,#7436,#7437,#7438,
#7439,#7440,#7441,#7442,#7443,#7444,#7445,#7446,#7447,#7448,#7449,#7450,
#7451,#7452,#7453,#7454,#7455,#7456,#7457,#7458,#7459,#7460,#7461,#7462,
#7463,#7464,#7465,#7466,#7467,#7468,#7469),.UNSPECIFIED.,.F.,.F.,(4,3,3,
3,3,3,3,3,3,3,3,3,3,3,3,3,3,3,3,3,3,3,3,3,4),(-0.177567088092164,-0.171205860781276,
-0.159841364771409,-0.153341448629585,-0.149825019995913,-0.137364180358316,
-0.13022989440132,-0.127506551868041,-0.125034870535725,-0.113089167658055,
-0.101422640254504,-0.0960446801741604,-0.0933155330928928,-0.091156106491866,
-0.0802898927023465,-0.0702536561145532,-0.0605144873326988,-0.0580925158103782,
-0.0469016452609415,-0.0358502799243893,-0.0306242181708044,-0.0277817060826135,
-0.0171983362218047,-0.00699990470760896,0.),.UNSPECIFIED.);
#126=B_SPLINE_CURVE_WITH_KNOTS('',3,(#7626,#7627,#7628,#7629,#7630,#7631,
#7632),.UNSPECIFIED.,.F.,.F.,(4,3,4),(32.531413144902,32.9929494494428,
33.9268444642796),.UNSPECIFIED.);
#127=B_SPLINE_CURVE_WITH_KNOTS('',3,(#7634,#7635,#7636,#7637,#7638,#7639,
#7640,#7641,#7642,#7643,#7644,#7645,#7646,#7647,#7648,#7649,#7650,#7651,
#7652,#7653,#7654,#7655,#7656,#7657,#7658,#7659,#7660,#7661,#7662,#7663,
#7664,#7665,#7666,#7667,#7668,#7669,#7670,#7671,#7672,#7673,#7674,#7675,
#7676,#7677,#7678,#7679,#7680,#7681,#7682,#7683,#7684,#7685,#7686,#7687,
#7688,#7689,#7690,#7691,#7692,#7693,#7694,#7695,#7696,#7697,#7698,#7699,
#7700,#7701,#7702,#7703,#7704,#7705,#7706,#7707,#7708,#7709),
 .UNSPECIFIED.,.F.,.F.,(4,3,3,3,3,3,3,3,3,3,3,3,3,3,3,3,3,3,3,3,3,3,3,3,
3,4),(-0.178587760439503,-0.173611807749089,-0.163438350924943,-0.158375685688331,
-0.155636582785503,-0.144832452490873,-0.140259718887796,-0.137183155499747,
-0.134746503227007,-0.12338758703633,-0.111954465066202,-0.106069912314992,
-0.103723896170116,-0.0922241531559212,-0.0806961340114311,-0.0752220431672022,
-0.0719210138736596,-0.0694880559864147,-0.0575218436472125,-0.0452790030681591,
-0.0393960367230259,-0.0368040370944524,-0.0343328909447597,-0.0216376025540469,
-0.00903060057598744,0.),.UNSPECIFIED.);
#128=B_SPLINE_CURVE_WITH_KNOTS('',3,(#7710,#7711,#7712,#7713,#7714,#7715,
#7716,#7717,#7718),.UNSPECIFIED.,.F.,.F.,(4,1,1,1,1,1,4),(10.374755377787,
11.3086503926238,12.3084367395766,13.3082230865294,14.3080094334822,15.307795780435,
15.707963267949),.UNSPECIFIED.);
#129=B_SPLINE_CURVE_WITH_KNOTS('',3,(#7724,#7725,#7726,#7727,#7728,#7729,
#7730,#7731,#7732,#7733,#7734,#7735,#7736,#7737,#7738,#7739,#7740,#7741,
#7742,#7743,#7744,#7745,#7746,#7747,#7748,#7749,#7750,#7751,#7752,#7753,
#7754,#7755,#7756,#7757,#7758,#7759,#7760,#7761,#7762,#7763,#7764,#7765,
#7766,#7767,#7768,#7769,#7770,#7771,#7772,#7773,#7774,#7775,#7776,#7777,
#7778,#7779,#7780,#7781,#7782,#7783,#7784,#7785,#7786,#7787,#7788,#7789,
#7790,#7791,#7792,#7793,#7794,#7795,#7796),.UNSPECIFIED.,.F.,.F.,(4,3,3,
3,3,3,3,3,3,3,3,3,3,3,3,3,3,3,3,3,3,3,3,3,4),(-0.177567088092158,-0.171205860781269,
-0.159841364771403,-0.153341449957138,-0.149825021408317,-0.137364182301213,
-0.130229896101354,-0.127506561096828,-0.125034891677152,-0.113089191744828,
-0.101422670425347,-0.0960447146844191,-0.0933157066615757,-0.0911564534648362,
-0.0802898927023405,-0.0702536561145479,-0.0605144868244642,-0.0580925152771776,
-0.0469016447884122,-0.0358502738466785,-0.0306242089636902,-0.0277817043216266,
-0.0171983284784898,-0.00699988795734099,0.),.UNSPECIFIED.);
#130=B_SPLINE_CURVE_WITH_KNOTS('',3,(#7799,#7800,#7801,#7802,#7803,#7804,
#7805,#7806),.UNSPECIFIED.,.F.,.F.,(4,1,1,1,1,4),(11.6163931973415,12.6161795442943,
13.6159658912471,14.6157522381999,15.6155385851527,15.707963267949),
 .UNSPECIFIED.);
#131=B_SPLINE_CURVE_WITH_KNOTS('',3,(#7963,#7964,#7965,#7966),
 .UNSPECIFIED.,.F.,.F.,(4,4),(-35.9923084903013,-35.5074966065054),
 .UNSPECIFIED.);
#132=B_SPLINE_CURVE_WITH_KNOTS('',3,(#8022,#8023,#8024,#8025,#8026,#8027,
#8028,#8029,#8030,#8031),.UNSPECIFIED.,.F.,.F.,(4,3,3,4),(-4.0928296534993,
-3.91485101570736,-2.93613826178052,-2.06974660785394),.UNSPECIFIED.);
#133=B_SPLINE_CURVE_WITH_KNOTS('',3,(#8034,#8035,#8036,#8037,#8038,#8039,
#8040),.UNSPECIFIED.,.F.,.F.,(4,3,4),(0.,0.97871275392684,1.11850960794444),
 .UNSPECIFIED.);
#134=B_SPLINE_CURVE_WITH_KNOTS('',3,(#8045,#8046,#8047,#8048,#8049,#8050,
#8051,#8052,#8053,#8054,#8055,#8056,#8057,#8058,#8059,#8060,#8061,#8062,
#8063,#8064,#8065,#8066),.UNSPECIFIED.,.F.,.F.,(4,3,3,3,3,3,3,4),(-10.3760149606789,
-9.7871275392684,-8.80841478534156,-7.82970203141472,-6.85098927748787,
-5.87227652356104,-4.8935637696342,-4.0928296534993),.UNSPECIFIED.);
#135=B_SPLINE_CURVE_WITH_KNOTS('',3,(#8067,#8068,#8069,#8070,#8071,#8072,
#8073,#8074,#8075,#8076,#8077,#8078,#8079,#8080,#8081,#8082,#8083,#8084,
#8085,#8086,#8087,#8088),.UNSPECIFIED.,.F.,.F.,(4,3,3,3,3,3,3,4),(1.11850960794444,
1.95742550785368,2.93613826178052,3.91485101570736,4.8935637696342,5.87227652356104,
6.85098927748788,7.40169491512403),.UNSPECIFIED.);
#136=B_SPLINE_CURVE_WITH_KNOTS('',3,(#8093,#8094,#8095,#8096,#8097,#8098,
#8099,#8100,#8101,#8102,#8103,#8104,#8105,#8106,#8107,#8108,#8109,#8110,
#8111,#8112,#8113,#8114,#8115,#8116,#8117),.UNSPECIFIED.,.F.,.F.,(4,3,3,
3,3,3,3,3,4),(-16.6592002678585,-16.6381168167563,-15.6594040628294,-14.6806913089026,
-13.7019785549758,-12.7232658010489,-11.7445530471221,-10.7658402931952,
-10.3760149606789),.UNSPECIFIED.);
#137=B_SPLINE_CURVE_WITH_KNOTS('',3,(#8118,#8119,#8120,#8121,#8122,#8123,
#8124,#8125,#8126,#8127,#8128,#8129,#8130,#8131,#8132,#8133,#8134,#8135,
#8136,#8137,#8138,#8139),.UNSPECIFIED.,.F.,.F.,(4,3,3,3,3,3,3,4),(7.40169491512403,
7.82970203141472,8.80841478534156,9.78712753926839,10.7658402931952,11.7445530471221,
12.7232658010489,13.6848802223036),.UNSPECIFIED.);
#138=B_SPLINE_CURVE_WITH_KNOTS('',3,(#8144,#8145,#8146,#8147,#8148,#8149,
#8150,#8151,#8152,#8153,#8154,#8155,#8156,#8157,#8158,#8159,#8160,#8161,
#8162,#8163,#8164,#8165),.UNSPECIFIED.,.F.,.F.,(4,3,3,3,3,3,3,4),(-22.9423855750381,
-22.5103933403173,-21.5316805863905,-20.5529678324636,-19.5742550785368,
-18.59554232461,-17.6168295706831,-16.6592002678585),.UNSPECIFIED.);
#139=B_SPLINE_CURVE_WITH_KNOTS('',3,(#8166,#8167,#8168,#8169,#8170,#8171,
#8172,#8173,#8174,#8175,#8176,#8177,#8178,#8179,#8180,#8181,#8182,#8183,
#8184,#8185,#8186,#8187,#8188,#8189,#8190),.UNSPECIFIED.,.F.,.F.,(4,3,3,
3,3,3,3,3,4),(13.6848802223036,13.7019785549758,14.6806913089026,15.6594040628294,
16.6381168167563,17.6168295706831,18.5955423246099,19.5742550785368,19.9680655294832),
 .UNSPECIFIED.);
#140=B_SPLINE_CURVE_WITH_KNOTS('',3,(#8195,#8196,#8197,#8198,#8199,#8200,
#8201,#8202,#8203,#8204,#8205,#8206,#8207,#8208,#8209,#8210,#8211,#8212,
#8213,#8214,#8215,#8216),.UNSPECIFIED.,.F.,.F.,(4,3,3,3,3,3,3,4),(-29.2255708822176,
-28.3826698638783,-27.4039571099515,-26.4252443560247,-25.4465316020978,
-24.467818848171,-23.4891060942441,-22.9423855750381),.UNSPECIFIED.);
#141=B_SPLINE_CURVE_WITH_KNOTS('',3,(#8217,#8218,#8219,#8220,#8221,#8222,
#8223,#8224,#8225,#8226,#8227,#8228,#8229,#8230,#8231,#8232,#8233,#8234,
#8235,#8236,#8237,#8238),.UNSPECIFIED.,.F.,.F.,(4,3,3,3,3,3,3,4),(19.9680655294832,
20.5529678324636,21.5316805863905,22.5103933403173,23.4891060942441,24.467818848171,
25.4465316020978,26.2512508366628),.UNSPECIFIED.);
#142=B_SPLINE_CURVE_WITH_KNOTS('',3,(#8244,#8245,#8246,#8247,#8248,#8249),
 .UNSPECIFIED.,.F.,.F.,(4,1,1,4),(40.8407044966673,40.9765162322549,41.9552289861817,
42.8216206401083),.UNSPECIFIED.);
#143=B_SPLINE_CURVE_WITH_KNOTS('',3,(#8252,#8253,#8254,#8255),
 .UNSPECIFIED.,.F.,.F.,(4,4),(40.8407044966673,41.5825019863375),
 .UNSPECIFIED.);
#144=B_SPLINE_CURVE_WITH_KNOTS('',3,(#8260,#8261,#8262,#8263,#8264,#8265,
#8266,#8267,#8268,#8269),.UNSPECIFIED.,.F.,.F.,(4,1,1,1,1,1,1,4),(34.5575191894877,
35.1042397086938,36.0829524626207,37.0616652165475,38.0403779704743,39.0190907244012,
39.997803478328,40.8407044966673),.UNSPECIFIED.);
#145=B_SPLINE_CURVE_WITH_KNOTS('',3,(#8270,#8271,#8272,#8273,#8274,#8275,
#8276,#8277,#8278,#8279,#8280),.UNSPECIFIED.,.F.,.F.,(4,1,1,1,1,1,1,1,4),
(34.5575191894877,34.7315127088496,35.7102254627764,36.6889382167033,37.6676509706301,
38.646363724557,39.6250764784838,40.6037892324106,40.8407044966673),
 .UNSPECIFIED.);
#146=B_SPLINE_CURVE_WITH_KNOTS('',3,(#8285,#8286,#8287,#8288,#8289,#8290,
#8291,#8292,#8293,#8294),.UNSPECIFIED.,.F.,.F.,(4,1,1,1,1,1,1,4),(28.2743338823081,
29.2319631851328,30.2106759390596,31.1893886929865,32.1681014469133,33.1468142008401,
34.125526954767,34.5575191894877),.UNSPECIFIED.);
#147=B_SPLINE_CURVE_WITH_KNOTS('',3,(#8295,#8296,#8297,#8298,#8299,#8300,
#8301,#8302,#8303,#8304),.UNSPECIFIED.,.F.,.F.,(4,1,1,1,1,1,1,4),(28.2743338823081,
28.8592361852886,29.8379489392154,30.8166616931422,31.7953744470691,32.7740872009959,
33.7527999549228,34.5575191894877),.UNSPECIFIED.);
#148=B_SPLINE_CURVE_WITH_KNOTS('',3,(#8309,#8310,#8311,#8312,#8313,#8314,
#8315,#8316,#8317,#8318,#8319),.UNSPECIFIED.,.F.,.F.,(4,1,1,1,1,1,1,1,4),
(21.9911485751285,22.3809739076449,23.3596866615717,24.3383994154986,25.3171121694254,
26.2958249233523,27.2745376772791,28.2532504312059,28.2743338823081),
 .UNSPECIFIED.);
#149=B_SPLINE_CURVE_WITH_KNOTS('',3,(#8320,#8321,#8322,#8323,#8324,#8325,
#8326,#8327,#8328,#8329,#8330),.UNSPECIFIED.,.F.,.F.,(4,1,1,1,1,1,1,1,4),
(21.9911485751285,22.0082469078007,22.9869596617275,23.9656724156544,24.9443851695812,
25.923097923508,26.9018106774349,27.8805234313617,28.2743338823081),
 .UNSPECIFIED.);
#150=B_SPLINE_CURVE_WITH_KNOTS('',3,(#8335,#8336,#8337,#8338,#8339,#8340,
#8341,#8342,#8343,#8344),.UNSPECIFIED.,.F.,.F.,(4,1,1,1,1,1,1,4),(15.707963267949,
16.5086973840839,17.4874101380107,18.4661228919375,19.4448356458644,20.4235483997912,
21.4022611537181,21.9911485751285),.UNSPECIFIED.);
#151=B_SPLINE_CURVE_WITH_KNOTS('',3,(#8345,#8346,#8347,#8348,#8349,#8350,
#8351,#8352,#8353,#8354),.UNSPECIFIED.,.F.,.F.,(4,1,1,1,1,1,1,4),(15.707963267949,
16.1359703842396,17.1146831381665,18.0933958920933,19.0721086460202,20.050821399947,
21.0295341538738,21.9911485751285),.UNSPECIFIED.);
#152=B_SPLINE_CURVE_WITH_KNOTS('',3,(#8504,#8505,#8506,#8507,#8508,#8509,
#8510,#8511,#8512,#8513,#8514,#8515,#8516,#8517,#8518,#8519,#8520,#8521,
#8522,#8523,#8524,#8525,#8526,#8527,#8528,#8529,#8530,#8531,#8532,#8533,
#8534,#8535,#8536,#8537,#8538,#8539,#8540,#8541,#8542,#8543,#8544,#8545,
#8546,#8547,#8548,#8549,#8550,#8551,#8552,#8553,#8554,#8555,#8556,#8557,
#8558,#8559,#8560,#8561,#8562,#8563,#8564,#8565,#8566,#8567,#8568,#8569,
#8570,#8571,#8572,#8573,#8574,#8575,#8576,#8577,#8578,#8579,#8580,#8581,
#8582,#8583,#8584,#8585),.UNSPECIFIED.,.F.,.F.,(4,3,3,3,3,3,3,3,3,3,3,3,
3,3,3,3,3,3,3,3,3,3,3,3,3,3,3,4),(-0.2263798216096,-0.212781296643935,-0.198764954499484,
-0.194348244024141,-0.19103137880398,-0.176141645981783,-0.166705260170101,
-0.163156832255381,-0.160273007739967,-0.145367395677056,-0.131314184979161,
-0.123648278606451,-0.12009892302652,-0.117708066911632,-0.104064816705108,
-0.100650559488324,-0.0880692395522834,-0.0819584633849732,-0.0783172232476268,
-0.0758731537810384,-0.0623358096117628,-0.0488821760013612,-0.0427719040011911,
-0.0392847357791446,-0.036186254561982,-0.0232691518627682,-0.0108090455882997,
0.),.UNSPECIFIED.);
#153=B_SPLINE_CURVE_WITH_KNOTS('',3,(#8586,#8587,#8588,#8589,#8590,#8591,
#8592,#8593,#8594,#8595,#8596,#8597,#8598,#8599,#8600,#8601,#8602,#8603,
#8604),.UNSPECIFIED.,.F.,.F.,(4,3,3,3,3,3,4),(26.2512508366628,26.4252443560247,
27.4039571099515,28.3826698638783,29.3613826178052,30.340095371732,31.2064870256586),
 .UNSPECIFIED.);
#154=B_SPLINE_CURVE_WITH_KNOTS('',3,(#8606,#8607,#8608,#8609,#8610,#8611,
#8612,#8613,#8614,#8615,#8616,#8617,#8618,#8619,#8620,#8621,#8622,#8623,
#8624,#8625,#8626,#8627,#8628,#8629,#8630,#8631,#8632,#8633,#8634,#8635,
#8636,#8637,#8638,#8639,#8640,#8641,#8642,#8643,#8644,#8645,#8646,#8647,
#8648,#8649,#8650,#8651,#8652,#8653,#8654,#8655,#8656,#8657,#8658,#8659,
#8660,#8661,#8662,#8663,#8664,#8665,#8666,#8667,#8668,#8669,#8670,#8671,
#8672,#8673,#8674,#8675,#8676,#8677,#8678),.UNSPECIFIED.,.F.,.F.,(4,3,3,
3,3,3,3,3,3,3,3,3,3,3,3,3,3,3,3,3,3,3,3,3,4),(-0.227523845437315,-0.216531207791372,
-0.203444509678888,-0.19917031778805,-0.186104896969351,-0.177062709219988,
-0.174032359669319,-0.160576649118607,-0.146770239359644,-0.138606747212735,
-0.134066956125942,-0.131712797600661,-0.117458517615624,-0.114116270772009,
-0.0998517369255078,-0.0931579911241419,-0.0906511125980258,-0.0764034745604488,
-0.0618085878200202,-0.0535532362928206,-0.0474979476179205,-0.0444986209948431,
-0.0293718149083609,-0.0143385875077465,0.),.UNSPECIFIED.);
#155=B_SPLINE_CURVE_WITH_KNOTS('',3,(#8679,#8680,#8681,#8682,#8683,#8684,
#8685,#8686,#8687),.UNSPECIFIED.,.F.,.F.,(4,1,1,1,1,1,4),(10.3760149606789,
11.2424066146055,12.2211193685323,13.1998321224591,14.178544876386,15.1572576303128,
15.707963267949),.UNSPECIFIED.);
#156=B_SPLINE_CURVE_WITH_KNOTS('',3,(#8693,#8694,#8695,#8696,#8697,#8698,
#8699,#8700,#8701,#8702,#8703,#8704,#8705,#8706,#8707,#8708,#8709,#8710,
#8711,#8712,#8713,#8714,#8715,#8716,#8717,#8718,#8719,#8720,#8721,#8722,
#8723,#8724,#8725,#8726,#8727,#8728,#8729,#8730,#8731,#8732,#8733,#8734,
#8735,#8736,#8737,#8738,#8739,#8740,#8741,#8742,#8743,#8744,#8745,#8746,
#8747,#8748,#8749,#8750,#8751,#8752,#8753,#8754,#8755,#8756,#8757,#8758,
#8759,#8760,#8761,#8762,#8763,#8764,#8765,#8766,#8767,#8768,#8769,#8770,
#8771,#8772,#8773,#8774),.UNSPECIFIED.,.F.,.F.,(4,3,3,3,3,3,3,3,3,3,3,3,
3,3,3,3,3,3,3,3,3,3,3,3,3,3,3,4),(-0.226379821609601,-0.212781296643936,
-0.198764954499484,-0.194348229390083,-0.191031373550795,-0.176141640284406,
-0.166705255184896,-0.163156771711209,-0.160272993847505,-0.14536738525771,
-0.131314163159309,-0.123648262241563,-0.120098829594509,-0.117707924800541,
-0.10406466589718,-0.100650559488325,-0.0880692395522841,-0.0819584595318643,
-0.0783172123161553,-0.0758731354163763,-0.062335788826532,-0.0488821638473745,
-0.0427718933664527,-0.0392847312763369,-0.0361862533404839,-0.0232691611782643,
-0.0108090724668815,0.),.UNSPECIFIED.);
#157=B_SPLINE_CURVE_WITH_KNOTS('',3,(#8777,#8778,#8779,#8780,#8781,#8782,
#8783,#8784),.UNSPECIFIED.,.F.,.F.,(4,1,1,1,1,4),(11.6151336144497,12.5938463683765,
13.5725591223033,14.5512718762302,15.529984630157,15.707963267949),
 .UNSPECIFIED.);
#158=B_SPLINE_CURVE_WITH_KNOTS('',3,(#8934,#8935,#8936,#8937,#8938,#8939,
#8940,#8941,#8942,#8943,#8944,#8945,#8946,#8947,#8948,#8949,#8950,#8951,
#8952,#8953,#8954,#8955,#8956,#8957,#8958,#8959,#8960,#8961,#8962,#8963,
#8964,#8965,#8966,#8967,#8968,#8969,#8970,#8971,#8972,#8973,#8974,#8975,
#8976,#8977,#8978,#8979,#8980,#8981,#8982,#8983,#8984,#8985,#8986,#8987,
#8988,#8989,#8990,#8991,#8992,#8993,#8994,#8995,#8996,#8997,#8998,#8999,
#9000,#9001,#9002,#9003,#9004,#9005,#9006),.UNSPECIFIED.,.F.,.F.,(4,3,3,
3,3,3,3,3,3,3,3,3,3,3,3,3,3,3,3,3,3,3,3,3,4),(-0.227523845437336,-0.216531207791394,
-0.203444511100821,-0.199170316873814,-0.186104887794658,-0.177062692209482,
-0.174032347803623,-0.160576629297939,-0.146770219866148,-0.138606732592615,
-0.134066934232983,-0.13171277086904,-0.117458491234212,-0.114116270772017,
-0.0998517369255152,-0.0931579924169406,-0.0906511134895252,-0.0764034708381965,
-0.0618085789631532,-0.0535532325040275,-0.0474979353490834,-0.0444986239739673,
-0.0293718142479027,-0.0143385961848834,0.),.UNSPECIFIED.);
#159=B_SPLINE_CURVE_WITH_KNOTS('',3,(#9007,#9008,#9009,#9010,#9011,#9012,
#9013,#9014,#9015,#9016,#9017,#9018,#9019,#9020,#9021,#9022),
 .UNSPECIFIED.,.F.,.F.,(4,3,3,3,3,4),(-33.2762336335125,-32.2975208795857,
-31.3188081256589,-30.340095371732,-29.3613826178052,-29.2255708822176),
 .UNSPECIFIED.);
#160=B_SPLINE_CURVE_WITH_KNOTS('',3,(#9138,#9139,#9140,#9141,#9142,#9143,
#9144,#9145,#9146,#9147,#9148,#9149,#9150,#9151,#9152,#9153,#9154,#9155,
#9156,#9157,#9158,#9159,#9160,#9161,#9162,#9163),.UNSPECIFIED.,.F.,.F.,
(4,2,2,2,2,2,2,2,2,2,2,2,4),(0.,0.0303730235339956,0.0607460470679912,0.0911072107271434,
0.121468374386296,0.151829538045448,0.1821907017046,0.212563725238596,0.242936748772591,
0.273309772306587,0.303682795840582,0.334043959499734,0.364405123158887),
 .UNSPECIFIED.);
#161=B_SPLINE_CURVE_WITH_KNOTS('',3,(#9164,#9165,#9166,#9167,#9168,#9169,
#9170,#9171,#9172,#9173),.UNSPECIFIED.,.F.,.F.,(4,2,2,2,4),(0.364405123158887,
0.394766286818039,0.425127450477191,0.455500474011187,0.485873497545182),
 .UNSPECIFIED.);
#162=B_SPLINE_CURVE_WITH_KNOTS('',3,(#9177,#9178,#9179,#9180,#9181,#9182,
#9183,#9184,#9185,#9186),.UNSPECIFIED.,.F.,.F.,(4,2,2,2,4),(0.,0.0303730235339955,
0.060746047067991,0.0911072107271433,0.121468374386295),.UNSPECIFIED.);
#163=B_SPLINE_CURVE_WITH_KNOTS('',3,(#9187,#9188,#9189,#9190,#9191,#9192,
#9193,#9194,#9195,#9196,#9197,#9198,#9199,#9200,#9201,#9202,#9203,#9204,
#9205,#9206,#9207,#9208,#9209,#9210,#9211,#9212),.UNSPECIFIED.,.F.,.F.,
(4,2,2,2,2,2,2,2,2,2,2,2,4),(0.121468374386295,0.151829538045448,0.1821907017046,
0.212563725238595,0.242936748772591,0.273309772306587,0.303682795840582,
0.334043959499734,0.364405123158887,0.394766286818039,0.425127450477191,
0.455500474011187,0.485873497545182),.UNSPECIFIED.);
#164=B_SPLINE_CURVE_WITH_KNOTS('',3,(#9398,#9399,#9400,#9401,#9402,#9403,
#9404,#9405,#9406,#9407),.UNSPECIFIED.,.F.,.F.,(4,3,3,4),(-4.09157007060746,
-3.99928089696595,-2.99946067272446,-2.06546402602173),.UNSPECIFIED.);
#165=B_SPLINE_CURVE_WITH_KNOTS('',3,(#9410,#9411,#9412,#9413,#9414,#9415,
#9416),.UNSPECIFIED.,.F.,.F.,(4,3,4),(0.,0.999820224241491,1.11548660900396),
 .UNSPECIFIED.);
#166=B_SPLINE_CURVE_WITH_KNOTS('',3,(#9421,#9422,#9423,#9424,#9425,#9426,
#9427,#9428,#9429,#9430,#9431,#9432,#9433,#9434,#9435,#9436,#9437,#9438,
#9439,#9440,#9441,#9442),.UNSPECIFIED.,.F.,.F.,(4,3,3,3,3,3,3,4),(-10.374755377787,
-9.99820224241487,-8.99838201817339,-7.9985617939319,-6.99874156969041,
-5.99892134544893,-4.99910112120744,-4.09157007060746),.UNSPECIFIED.);
#167=B_SPLINE_CURVE_WITH_KNOTS('',3,(#9443,#9444,#9445,#9446,#9447,#9448,
#9449,#9450,#9451,#9452,#9453,#9454,#9455,#9456,#9457,#9458,#9459,#9460,
#9461,#9462,#9463,#9464),.UNSPECIFIED.,.F.,.F.,(4,3,3,3,3,3,3,4),(1.11548660900396,
1.99964044848298,2.99946067272447,3.99928089696595,4.99910112120744,5.99892134544892,
6.99874156969041,7.39867191618355),.UNSPECIFIED.);
#168=B_SPLINE_CURVE_WITH_KNOTS('',3,(#9469,#9470,#9471,#9472,#9473,#9474,
#9475,#9476,#9477,#9478,#9479,#9480,#9481,#9482,#9483,#9484,#9485,#9486,
#9487,#9488,#9489,#9490),.UNSPECIFIED.,.F.,.F.,(4,3,3,3,3,3,3,4),(-16.6579406849666,
-15.9971235878638,-14.9973033636223,-13.9974831393808,-12.9976629151393,
-11.9978426908978,-10.9980224666564,-10.374755377787),.UNSPECIFIED.);
#169=B_SPLINE_CURVE_WITH_KNOTS('',3,(#9491,#9492,#9493,#9494,#9495,#9496,
#9497,#9498,#9499,#9500,#9501,#9502,#9503,#9504,#9505,#9506,#9507,#9508,
#9509,#9510,#9511,#9512),.UNSPECIFIED.,.F.,.F.,(4,3,3,3,3,3,3,4),(7.39867191618355,
7.9985617939319,8.99838201817339,9.99820224241487,10.9980224666564,11.9978426908979,
12.9976629151393,13.6818572233631),.UNSPECIFIED.);
#170=B_SPLINE_CURVE_WITH_KNOTS('',3,(#9517,#9518,#9519,#9520,#9521,#9522,
#9523,#9524,#9525,#9526,#9527,#9528,#9529,#9530,#9531,#9532,#9533,#9534,
#9535,#9536,#9537,#9538),.UNSPECIFIED.,.F.,.F.,(4,3,3,3,3,3,3,4),(-22.9411259921462,
-21.9960449333127,-20.9962247090712,-19.9964044848298,-18.9965842605883,
-17.9967640363468,-16.9969438121053,-16.6579406849666),.UNSPECIFIED.);
#171=B_SPLINE_CURVE_WITH_KNOTS('',3,(#9539,#9540,#9541,#9542,#9543,#9544,
#9545,#9546,#9547,#9548,#9549,#9550,#9551,#9552,#9553,#9554,#9555,#9556,
#9557,#9558,#9559,#9560),.UNSPECIFIED.,.F.,.F.,(4,3,3,3,3,3,3,4),(13.6818572233631,
13.9974831393808,14.9973033636223,15.9971235878638,16.9969438121053,17.9967640363468,
18.9965842605883,19.9650425305427),.UNSPECIFIED.);
#172=B_SPLINE_CURVE_WITH_KNOTS('',3,(#9565,#9566,#9567,#9568,#9569,#9570,
#9571,#9572,#9573,#9574,#9575,#9576,#9577,#9578,#9579,#9580,#9581,#9582,
#9583,#9584,#9585,#9586,#9587,#9588,#9589),.UNSPECIFIED.,.F.,.F.,(4,3,3,
3,3,3,3,3,4),(-29.2243112993258,-28.9947865030031,-27.9949662787616,-26.9951460545202,
-25.9953258302787,-24.9955056060372,-23.9956853817957,-22.9958651575542,
-22.9411259921462),.UNSPECIFIED.);
#173=B_SPLINE_CURVE_WITH_KNOTS('',3,(#9590,#9591,#9592,#9593,#9594,#9595,
#9596,#9597,#9598,#9599,#9600,#9601,#9602,#9603,#9604,#9605,#9606,#9607,
#9608,#9609,#9610,#9611,#9612,#9613,#9614),.UNSPECIFIED.,.F.,.F.,(4,3,3,
3,3,3,3,3,4),(19.9650425305427,19.9964044848298,20.9962247090712,21.9960449333127,
22.9958651575542,23.9956853817957,24.9955056060372,25.9953258302787,26.2482278377223),
 .UNSPECIFIED.);
#174=B_SPLINE_CURVE_WITH_KNOTS('',3,(#9619,#9620,#9621,#9622,#9623,#9624,
#9625,#9626,#9627,#9628,#9629,#9630,#9631,#9632,#9633,#9634,#9635,#9636,
#9637,#9638,#9639,#9640),.UNSPECIFIED.,.F.,.F.,(4,3,3,3,3,3,3,4),(-35.5074966065054,
-34.9937078484521,-33.9938876242106,-32.9940673999691,-31.9942471757276,
-30.9944269514861,-29.9946067272446,-29.2243112993258),.UNSPECIFIED.);
#175=B_SPLINE_CURVE_WITH_KNOTS('',3,(#9641,#9642,#9643,#9644,#9645,#9646,
#9647,#9648,#9649,#9650,#9651,#9652,#9653,#9654,#9655,#9656,#9657,#9658,
#9659,#9660,#9661,#9662),.UNSPECIFIED.,.F.,.F.,(4,3,3,3,3,3,3,4),(26.2482278377223,
26.9951460545202,27.9949662787616,28.9947865030031,29.9946067272446,30.9944269514861,
31.9942471757276,32.5314131449019),.UNSPECIFIED.);
#176=B_SPLINE_CURVE_WITH_KNOTS('',3,(#9667,#9668,#9669,#9670,#9671,#9672,
#9673,#9674,#9675,#9676,#9677,#9678,#9679,#9680,#9681,#9682,#9683,#9684,
#9685,#9686,#9687,#9688),.UNSPECIFIED.,.F.,.F.,(4,3,3,3,3,3,3,4),(-41.790681913685,
-40.992629193901,-39.9928089696595,-38.992988745418,-37.9931685211765,-36.993348296935,
-35.9935280726936,-35.5074966065054),.UNSPECIFIED.);
#177=B_SPLINE_CURVE_WITH_KNOTS('',3,(#9689,#9690,#9691,#9692,#9693,#9694,
#9695,#9696,#9697,#9698,#9699,#9700,#9701,#9702,#9703,#9704,#9705,#9706,
#9707,#9708,#9709,#9710),.UNSPECIFIED.,.F.,.F.,(4,3,3,3,3,3,3,4),(32.5314131449019,
32.9940673999691,33.9938876242106,34.9937078484521,35.9935280726935,36.993348296935,
37.9931685211765,38.8145984520815),.UNSPECIFIED.);
#178=B_SPLINE_CURVE_WITH_KNOTS('',3,(#9715,#9716,#9717,#9718,#9719,#9720,
#9721,#9722,#9723,#9724,#9725,#9726,#9727,#9728,#9729,#9730,#9731,#9732,
#9733,#9734,#9735,#9736,#9737,#9738,#9739),.UNSPECIFIED.,.F.,.F.,(4,3,3,
3,3,3,3,3,4),(-48.0738672208646,-47.9913707635914,-46.9915505393499,-45.9917303151084,
-44.9919100908669,-43.9920898666255,-42.992269642384,-41.9924494181425,
-41.790681913685),.UNSPECIFIED.);
#179=B_SPLINE_CURVE_WITH_KNOTS('',3,(#9740,#9741,#9742,#9743,#9744,#9745,
#9746,#9747,#9748,#9749,#9750,#9751,#9752,#9753,#9754,#9755,#9756,#9757,
#9758,#9759,#9760,#9761,#9762,#9763,#9764),.UNSPECIFIED.,.F.,.F.,(4,3,3,
3,3,3,3,3,4),(38.8145984520815,38.992988745418,39.9928089696595,40.992629193901,
41.9924494181425,42.992269642384,43.9920898666254,44.9919100908669,45.0977837592611),
 .UNSPECIFIED.);
#180=B_SPLINE_CURVE_WITH_KNOTS('',3,(#9769,#9770,#9771,#9772,#9773,#9774,
#9775,#9776,#9777,#9778,#9779,#9780,#9781,#9782,#9783,#9784,#9785,#9786,
#9787,#9788,#9789,#9790),.UNSPECIFIED.,.F.,.F.,(4,3,3,3,3,3,3,4),(-54.3570525280442,
-53.9902921090403,-52.9904718847989,-51.9906516605573,-50.9908314363159,
-49.9910112120744,-48.9911909878329,-48.0738672208646),.UNSPECIFIED.);
#181=B_SPLINE_CURVE_WITH_KNOTS('',3,(#9791,#9792,#9793,#9794,#9795,#9796,
#9797,#9798,#9799,#9800,#9801,#9802,#9803,#9804,#9805,#9806,#9807,#9808,
#9809,#9810,#9811,#9812),.UNSPECIFIED.,.F.,.F.,(4,3,3,3,3,3,3,4),(45.0977837592611,
45.9917303151084,46.9915505393499,47.9913707635914,48.9911909878329,49.9910112120744,
50.9908314363159,51.3809690664407),.UNSPECIFIED.);
#182=B_SPLINE_CURVE_WITH_KNOTS('',3,(#9817,#9818,#9819,#9820,#9821,#9822,
#9823,#9824,#9825,#9826,#9827,#9828,#9829,#9830,#9831,#9832,#9833,#9834,
#9835,#9836,#9837,#9838),.UNSPECIFIED.,.F.,.F.,(4,3,3,3,3,3,3,4),(-60.6402378352238,
-59.9892134544893,-58.9893932302478,-57.9895730060063,-56.9897527817648,
-55.9899325575233,-54.9901123332818,-54.3570525280442),.UNSPECIFIED.);
#183=B_SPLINE_CURVE_WITH_KNOTS('',3,(#9839,#9840,#9841,#9842,#9843,#9844,
#9845,#9846,#9847,#9848,#9849,#9850,#9851,#9852,#9853,#9854,#9855,#9856,
#9857,#9858,#9859,#9860),.UNSPECIFIED.,.F.,.F.,(4,3,3,3,3,3,3,4),(51.3809690664407,
51.9906516605574,52.9904718847988,53.9902921090403,54.9901123332818,55.9899325575233,
56.9897527817648,57.6641543736203),.UNSPECIFIED.);
#184=B_SPLINE_CURVE_WITH_KNOTS('',3,(#9865,#9866,#9867,#9868,#9869,#9870,
#9871,#9872,#9873,#9874,#9875,#9876,#9877,#9878,#9879,#9880,#9881,#9882,
#9883,#9884,#9885,#9886),.UNSPECIFIED.,.F.,.F.,(4,3,3,3,3,3,3,4),(-66.9234231424034,
-65.9881347999382,-64.9883145756967,-63.9884943514552,-62.9886741272137,
-61.9888539029722,-60.9890336787308,-60.6402378352238),.UNSPECIFIED.);
#185=B_SPLINE_CURVE_WITH_KNOTS('',3,(#9887,#9888,#9889,#9890,#9891,#9892,
#9893,#9894,#9895,#9896,#9897,#9898,#9899,#9900,#9901,#9902,#9903,#9904,
#9905,#9906,#9907,#9908),.UNSPECIFIED.,.F.,.F.,(4,3,3,3,3,3,3,4),(57.6641543736203,
57.9895730060063,58.9893932302477,59.9892134544892,60.9890336787307,61.9888539029722,
62.9886741272137,63.9473396807999),.UNSPECIFIED.);
#186=B_SPLINE_CURVE_WITH_KNOTS('',3,(#9913,#9914,#9915,#9916,#9917,#9918,
#9919,#9920,#9921,#9922,#9923,#9924,#9925,#9926,#9927,#9928,#9929,#9930,
#9931,#9932,#9933,#9934,#9935,#9936,#9937),.UNSPECIFIED.,.F.,.F.,(4,3,3,
3,3,3,3,3,4),(-73.2066084495829,-72.9868763696286,-71.9870561453871,-70.9872359211456,
-69.9874156969041,-68.9875954726626,-67.9877752484212,-66.9879550241797,
-66.9234231424034),.UNSPECIFIED.);
#187=B_SPLINE_CURVE_WITH_KNOTS('',3,(#9938,#9939,#9940,#9941,#9942,#9943,
#9944,#9945,#9946,#9947,#9948,#9949,#9950,#9951,#9952,#9953,#9954,#9955,
#9956,#9957,#9958,#9959,#9960,#9961,#9962),.UNSPECIFIED.,.F.,.F.,(4,3,3,
3,3,3,3,3,4),(63.9473396807999,63.9884943514552,64.9883145756967,65.9881347999382,
66.9879550241797,67.9877752484211,68.9875954726626,69.9874156969041,70.2305249879795),
 .UNSPECIFIED.);
#188=B_SPLINE_CURVE_WITH_KNOTS('',3,(#9968,#9969,#9970,#9971,#9972,#9973),
 .UNSPECIFIED.,.F.,.F.,(4,1,1,4),(84.8230016469244,85.6030897912115,86.602910015453,
87.5369066621557),.UNSPECIFIED.);
#189=B_SPLINE_CURVE_WITH_KNOTS('',3,(#9976,#9977,#9978,#9979,#9980),
 .UNSPECIFIED.,.F.,.F.,(4,1,4),(84.8230016469244,85.2954486183598,86.2952688426013),
 .UNSPECIFIED.);
#190=B_SPLINE_CURVE_WITH_KNOTS('',3,(#9985,#9986,#9987,#9988,#9989,#9990,
#9991,#9992,#9993,#9994,#9995),.UNSPECIFIED.,.F.,.F.,(4,1,1,1,1,1,1,1,4),
(78.5398163397448,78.6043482215211,79.6041684457626,80.6039886700041,81.6038088942456,
82.6036291184871,83.6034493427286,84.60326956697,84.8230016469244),
 .UNSPECIFIED.);
#191=B_SPLINE_CURVE_WITH_KNOTS('',3,(#9996,#9997,#9998,#9999,#10000,#10001,
#10002,#10003,#10004,#10005),.UNSPECIFIED.,.F.,.F.,(4,1,1,1,1,1,1,4),(78.5398163397448,
79.2965272729109,80.2963474971524,81.2961677213939,82.2959879456354,83.2958081698768,
84.2956283941183,84.8230016469244),.UNSPECIFIED.);
#192=B_SPLINE_CURVE_WITH_KNOTS('',3,(#10010,#10011,#10012,#10013,#10014,
#10015,#10016,#10017,#10018,#10019),.UNSPECIFIED.,.F.,.F.,(4,1,1,1,1,1,
1,4),(72.2566310325652,72.6054268760722,73.6052471003137,74.6050673245552,
75.6048875487966,76.6047077730381,77.6045279972796,78.5398163397448),
 .UNSPECIFIED.);
#193=B_SPLINE_CURVE_WITH_KNOTS('',3,(#10020,#10021,#10022,#10023,#10024,
#10025,#10026,#10027,#10028,#10029,#10030),.UNSPECIFIED.,.F.,.F.,(4,1,1,
1,1,1,1,1,4),(72.2566310325652,72.2977857032205,73.297605927462,74.2974261517035,
75.297246375945,76.2970666001864,77.2968868244279,78.2967070486694,78.5398163397448),
 .UNSPECIFIED.);
#194=B_SPLINE_CURVE_WITH_KNOTS('',3,(#10035,#10036,#10037,#10038,#10039,
#10040,#10041,#10042,#10043,#10044),.UNSPECIFIED.,.F.,.F.,(4,1,1,1,1,1,
1,4),(65.9734457253856,66.6065055306233,67.6063257548647,68.6061459791062,
69.6059662033477,70.6057864275892,71.6056066518307,72.2566310325652),
 .UNSPECIFIED.);
#195=B_SPLINE_CURVE_WITH_KNOTS('',3,(#10045,#10046,#10047,#10048,#10049,
#10050,#10051,#10052,#10053,#10054),.UNSPECIFIED.,.F.,.F.,(4,1,1,1,1,1,
1,4),(65.9734457253856,66.2988643577716,67.298684582013,68.2985048062545,
69.298325030496,70.2981452547375,71.297965478979,72.2566310325652),
 .UNSPECIFIED.);
#196=B_SPLINE_CURVE_WITH_KNOTS('',3,(#10059,#10060,#10061,#10062,#10063,
#10064,#10065,#10066,#10067,#10068),.UNSPECIFIED.,.F.,.F.,(4,1,1,1,1,1,
1,4),(59.690260418206,60.6075841851743,61.6074044094158,62.6072246336573,
63.6070448578988,64.6068650821403,65.6066853063818,65.9734457253856),
 .UNSPECIFIED.);
#197=B_SPLINE_CURVE_WITH_KNOTS('',3,(#10069,#10070,#10071,#10072,#10073,
#10074,#10075,#10076,#10077,#10078),.UNSPECIFIED.,.F.,.F.,(4,1,1,1,1,1,
1,4),(59.690260418206,60.2999430123226,61.2997632365641,62.2995834608056,
63.2994036850471,64.2992239092886,65.2990441335301,65.9734457253856),
 .UNSPECIFIED.);
#198=B_SPLINE_CURVE_WITH_KNOTS('',3,(#10083,#10084,#10085,#10086,#10087,
#10088,#10089,#10090,#10091,#10092,#10093),.UNSPECIFIED.,.F.,.F.,(4,1,1,
1,1,1,1,1,4),(53.4070751110265,53.6088426154839,54.6086628397254,55.6084830639669,
56.6083032882084,57.6081235124499,58.6079437366914,59.6077639609328,59.690260418206),
 .UNSPECIFIED.);
#199=B_SPLINE_CURVE_WITH_KNOTS('',3,(#10094,#10095,#10096,#10097,#10098,
#10099,#10100,#10101,#10102,#10103),.UNSPECIFIED.,.F.,.F.,(4,1,1,1,1,1,
1,4),(53.4070751110264,54.3010216668737,55.3008418911152,56.3006621153567,
57.3004823395982,58.3003025638397,59.3001227880811,59.690260418206),
 .UNSPECIFIED.);
#200=B_SPLINE_CURVE_WITH_KNOTS('',3,(#10108,#10109,#10110,#10111,#10112,
#10113,#10114,#10115,#10116,#10117),.UNSPECIFIED.,.F.,.F.,(4,1,1,1,1,1,
1,4),(47.1238898038469,47.609921270035,48.6097414942765,49.609561718518,
50.6093819427595,51.6092021670009,52.6090223912424,53.4070751110265),
 .UNSPECIFIED.);
#201=B_SPLINE_CURVE_WITH_KNOTS('',3,(#10118,#10119,#10120,#10121,#10122,
#10123,#10124,#10125,#10126,#10127,#10128),.UNSPECIFIED.,.F.,.F.,(4,1,1,
1,1,1,1,1,4),(47.1238898038468,47.3022800971833,48.3021003214248,49.3019205456663,
50.3017407699078,51.3015609941492,52.3013812183907,53.3012014426322,53.4070751110264),
 .UNSPECIFIED.);
#202=B_SPLINE_CURVE_WITH_KNOTS('',3,(#10133,#10134,#10135,#10136,#10137,
#10138,#10139,#10140,#10141,#10142),.UNSPECIFIED.,.F.,.F.,(4,1,1,1,1,1,
1,4),(40.8407044966673,41.6109999245861,42.6108201488276,43.610640373069,
44.6104605973105,45.610280821552,46.6101010457935,47.1238898038469),
 .UNSPECIFIED.);
#203=B_SPLINE_CURVE_WITH_KNOTS('',3,(#10143,#10144,#10145,#10146,#10147,
#10148,#10149,#10150,#10151,#10152),.UNSPECIFIED.,.F.,.F.,(4,1,1,1,1,1,
1,4),(40.8407044966673,41.3033587517344,42.3031789759759,43.3029992002174,
44.3028194244588,45.3026396487003,46.3024598729418,47.1238898038468),
 .UNSPECIFIED.);
#204=B_SPLINE_CURVE_WITH_KNOTS('',3,(#10157,#10158,#10159,#10160,#10161,
#10162,#10163,#10164,#10165,#10166,#10167),.UNSPECIFIED.,.F.,.F.,(4,1,1,
1,1,1,1,1,4),(34.5575191894877,34.6122583548957,35.6120785791371,36.6118988033786,
37.6117190276201,38.6115392518616,39.6113594761031,40.6111797003446,40.8407044966673),
 .UNSPECIFIED.);
#205=B_SPLINE_CURVE_WITH_KNOTS('',3,(#10168,#10169,#10170,#10171,#10172,
#10173,#10174,#10175,#10176,#10177),.UNSPECIFIED.,.F.,.F.,(4,1,1,1,1,1,
1,4),(34.5575191894877,35.3044374062855,36.3042576305269,37.3040778547684,
38.3038980790099,39.3037183032514,40.3035385274929,40.8407044966673),
 .UNSPECIFIED.);
#206=B_SPLINE_CURVE_WITH_KNOTS('',3,(#10182,#10183,#10184,#10185,#10186,
#10187,#10188,#10189,#10190,#10191),.UNSPECIFIED.,.F.,.F.,(4,1,1,1,1,1,
1,4),(28.2743338823081,28.6133370094467,29.6131572336882,30.6129774579297,
31.6127976821712,32.6126179064127,33.6124381306542,34.5575191894877),
 .UNSPECIFIED.);
#207=B_SPLINE_CURVE_WITH_KNOTS('',3,(#10192,#10193,#10194,#10195,#10196,
#10197,#10198,#10199,#10200,#10201,#10202),.UNSPECIFIED.,.F.,.F.,(4,1,1,
1,1,1,1,1,4),(28.2743338823081,28.305695836595,29.3055160608365,30.305336285078,
31.3051565093195,32.304976733561,33.3047969578025,34.304617182044,34.5575191894877),
 .UNSPECIFIED.);
#208=B_SPLINE_CURVE_WITH_KNOTS('',3,(#10207,#10208,#10209,#10210,#10211,
#10212,#10213,#10214,#10215,#10216),.UNSPECIFIED.,.F.,.F.,(4,1,1,1,1,1,
1,4),(21.9911485751285,22.6144156639978,23.6142358882393,24.6140561124808,
25.6138763367223,26.6136965609638,27.6135167852052,28.2743338823081),
 .UNSPECIFIED.);
#209=B_SPLINE_CURVE_WITH_KNOTS('',3,(#10217,#10218,#10219,#10220,#10221,
#10222,#10223,#10224,#10225,#10226),.UNSPECIFIED.,.F.,.F.,(4,1,1,1,1,1,
1,4),(21.9911485751285,22.3067744911461,23.3065947153876,24.3064149396291,
25.3062351638706,26.3060553881121,27.3058756123536,28.2743338823081),
 .UNSPECIFIED.);
#210=B_SPLINE_CURVE_WITH_KNOTS('',3,(#10231,#10232,#10233,#10234,#10235,
#10236,#10237,#10238,#10239,#10240),.UNSPECIFIED.,.F.,.F.,(4,1,1,1,1,1,
1,4),(15.7079632679489,16.6154943185489,17.6153145427904,18.6151347670319,
19.6149549912733,20.6147752155148,21.6145954397563,21.9911485751285),
 .UNSPECIFIED.);
#211=B_SPLINE_CURVE_WITH_KNOTS('',3,(#10241,#10242,#10243,#10244,#10245,
#10246,#10247,#10248,#10249,#10250),.UNSPECIFIED.,.F.,.F.,(4,1,1,1,1,1,
1,4),(15.7079632679489,16.3078531456972,17.3076733699387,18.3074935941802,
19.3073138184217,20.3071340426631,21.3069542669046,21.9911485751285),
 .UNSPECIFIED.);
#212=B_SPLINE_CURVE_WITH_KNOTS('',3,(#10576,#10577,#10578,#10579,#10580,
#10581,#10582,#10583,#10584,#10585,#10586,#10587,#10588,#10589,#10590,#10591,
#10592,#10593,#10594,#10595,#10596,#10597,#10598,#10599,#10600,#10601,#10602,
#10603,#10604,#10605,#10606,#10607,#10608,#10609,#10610,#10611,#10612,#10613,
#10614,#10615,#10616,#10617,#10618,#10619,#10620,#10621,#10622,#10623,#10624,
#10625,#10626,#10627,#10628,#10629,#10630,#10631,#10632,#10633,#10634,#10635,
#10636,#10637,#10638,#10639,#10640,#10641,#10642,#10643,#10644,#10645,#10646,
#10647,#10648),.UNSPECIFIED.,.F.,.F.,(4,3,3,3,3,3,3,3,3,3,3,3,3,3,3,3,3,
3,3,3,3,3,3,3,4),(-0.177567088092159,-0.171212382832697,-0.159847434768505,
-0.153345817358462,-0.149826690596105,-0.137365842819437,-0.130231712256903,
-0.127511381423288,-0.125045141948771,-0.113099295309258,-0.101432568059643,
-0.0960567658811824,-0.0933691339394849,-0.0912510517173706,-0.0802927983191652,
-0.0702561985292696,-0.0605201785902624,-0.0580933766023054,-0.0469024983635594,
-0.0358510772443959,-0.0306253907821055,-0.027781893072329,-0.0171984826633998,
-0.00699999386689098,0.),.UNSPECIFIED.);
#213=B_SPLINE_CURVE_WITH_KNOTS('',3,(#10649,#10650,#10651,#10652,#10653,
#10654,#10655,#10656,#10657,#10658,#10659,#10660,#10661,#10662,#10663,#10664,
#10665,#10666,#10667),.UNSPECIFIED.,.F.,.F.,(4,3,3,3,3,3,4),(70.2305249879795,
70.9872359211456,71.9870561453871,72.9868763696286,73.9866965938701,74.9865168181115,
75.9205134648143),.UNSPECIFIED.);
#214=B_SPLINE_CURVE_WITH_KNOTS('',3,(#10669,#10670,#10671,#10672,#10673,
#10674,#10675,#10676,#10677,#10678,#10679,#10680,#10681,#10682,#10683,#10684,
#10685,#10686,#10687,#10688,#10689,#10690,#10691,#10692,#10693,#10694,#10695,
#10696,#10697,#10698,#10699,#10700,#10701,#10702,#10703,#10704,#10705,#10706,
#10707,#10708,#10709,#10710,#10711,#10712,#10713,#10714,#10715,#10716,#10717,
#10718,#10719,#10720,#10721,#10722,#10723,#10724,#10725,#10726,#10727,#10728,
#10729,#10730,#10731,#10732,#10733,#10734,#10735,#10736,#10737,#10738,#10739,
#10740,#10741,#10742,#10743,#10744),.UNSPECIFIED.,.F.,.F.,(4,3,3,3,3,3,
3,3,3,3,3,3,3,3,3,3,3,3,3,3,3,3,3,3,3,4),(-0.178587760439503,-0.173616952387545,
-0.16344322079987,-0.158392709244495,-0.155639480293815,-0.144835430750113,
-0.140266276985465,-0.137197164839716,-0.134748989799821,-0.123390106745024,
-0.111956963305991,-0.106074580361539,-0.103726213045244,-0.0922270996861484,
-0.0806987122253798,-0.0752226293283448,-0.0719230426967008,-0.0694885266869695,
-0.0575223232848203,-0.0452794892284,-0.0393966780719834,-0.0368033977106405,
-0.0343327348534217,-0.021637442866742,-0.00903041240735042,0.),
 .UNSPECIFIED.);
#215=B_SPLINE_CURVE_WITH_KNOTS('',3,(#10745,#10746,#10747,#10748,#10749,
#10750,#10751,#10752,#10753),.UNSPECIFIED.,.F.,.F.,(4,1,1,1,1,1,4),(10.374755377787,
11.3087520244898,12.3085722487312,13.3083924729727,14.3082126972142,15.3080329214557,
15.7079632679489),.UNSPECIFIED.);
#216=B_SPLINE_CURVE_WITH_KNOTS('',3,(#10759,#10760,#10761,#10762,#10763,
#10764,#10765,#10766,#10767,#10768,#10769,#10770,#10771,#10772,#10773,#10774,
#10775,#10776,#10777,#10778,#10779,#10780,#10781,#10782,#10783,#10784,#10785,
#10786,#10787,#10788,#10789,#10790,#10791,#10792,#10793,#10794,#10795,#10796,
#10797,#10798,#10799,#10800,#10801,#10802,#10803,#10804,#10805,#10806,#10807,
#10808,#10809,#10810,#10811,#10812,#10813,#10814,#10815,#10816,#10817,#10818,
#10819,#10820,#10821,#10822,#10823,#10824,#10825,#10826,#10827,#10828,#10829,
#10830,#10831),.UNSPECIFIED.,.F.,.F.,(4,3,3,3,3,3,3,3,3,3,3,3,3,3,3,3,3,
3,3,3,3,3,3,3,4),(-0.177567088092151,-0.171212382832686,-0.159847434768495,
-0.153345816518774,-0.149826689698261,-0.13736584158518,-0.130231711176927,
-0.127511375561844,-0.125045128746514,-0.113099280232028,-0.101432549106587,
-0.0960567442113712,-0.0933690332193806,-0.0912508938372308,-0.080292798319158,
-0.0702561985292632,-0.060520178916519,-0.05809337693984,-0.04690249865854,
-0.0358510810988072,-0.0306253966205261,-0.0277818941871718,-0.0171984875775208,
-0.00700000450395239,0.),.UNSPECIFIED.);
#217=B_SPLINE_CURVE_WITH_KNOTS('',3,(#10834,#10835,#10836,#10837,#10838,
#10839,#10840,#10841),.UNSPECIFIED.,.F.,.F.,(4,1,1,1,1,4),(11.6163931973414,
12.6162134215829,13.6160336458244,14.6158538700659,15.6156740943074,15.7079632679489),
 .UNSPECIFIED.);
#218=B_SPLINE_CURVE_WITH_KNOTS('',3,(#11167,#11168,#11169,#11170,#11171,
#11172,#11173,#11174,#11175,#11176,#11177,#11178,#11179,#11180,#11181,#11182,
#11183,#11184,#11185,#11186,#11187,#11188,#11189,#11190,#11191,#11192,#11193,
#11194,#11195,#11196,#11197,#11198,#11199,#11200,#11201,#11202,#11203,#11204,
#11205,#11206,#11207,#11208,#11209,#11210,#11211,#11212,#11213,#11214,#11215,
#11216,#11217,#11218,#11219,#11220,#11221,#11222,#11223,#11224,#11225,#11226,
#11227,#11228,#11229,#11230,#11231,#11232,#11233,#11234,#11235,#11236,#11237,
#11238,#11239,#11240,#11241,#11242),.UNSPECIFIED.,.F.,.F.,(4,3,3,3,3,3,
3,3,3,3,3,3,3,3,3,3,3,3,3,3,3,3,3,3,3,4),(-0.178587760439493,-0.173616952387535,
-0.163443220799861,-0.158392707607725,-0.155639479461434,-0.144835427076733,
-0.140266268421766,-0.13719714418731,-0.134748985506781,-0.123390101386577,
-0.111956958245561,-0.10607457323289,-0.103726209196408,-0.0922270996861424,
-0.0806987122253746,-0.0752226294429386,-0.0719230446435219,-0.0694885274270723,
-0.0575223226511971,-0.0452794871814101,-0.0393966756816979,-0.0368033999362885,
-0.0343327356829297,-0.0216374425574168,-0.00903041530155625,0.),
 .UNSPECIFIED.);
#219=B_SPLINE_CURVE_WITH_KNOTS('',3,(#11243,#11244,#11245,#11246,#11247,
#11248,#11249,#11250,#11251,#11252,#11253,#11254,#11255,#11256,#11257,#11258),
 .UNSPECIFIED.,.F.,.F.,(4,3,3,3,3,4),(-77.985977490836,-76.9861572665945,
-75.986337042353,-74.9865168181116,-73.9866965938701,-73.2066084495829),
 .UNSPECIFIED.);
#220=(
BOUNDED_CURVE()
B_SPLINE_CURVE(2,(#6614,#6615,#6616),.UNSPECIFIED.,.F.,.F.)
B_SPLINE_CURVE_WITH_KNOTS((3,3),(0.,0.0309504086115576),.UNSPECIFIED.)
CURVE()
GEOMETRIC_REPRESENTATION_ITEM()
RATIONAL_B_SPLINE_CURVE((1.,1.,1.))
REPRESENTATION_ITEM('')
);
#221=(
BOUNDED_CURVE()
B_SPLINE_CURVE(2,(#6620,#6621,#6622),.UNSPECIFIED.,.F.,.F.)
B_SPLINE_CURVE_WITH_KNOTS((3,3),(0.,0.0289695421536074),.UNSPECIFIED.)
CURVE()
GEOMETRIC_REPRESENTATION_ITEM()
RATIONAL_B_SPLINE_CURVE((1.,1.,1.))
REPRESENTATION_ITEM('')
);
#222=(
BOUNDED_CURVE()
B_SPLINE_CURVE(2,(#6626,#6627,#6628),.UNSPECIFIED.,.F.,.F.)
B_SPLINE_CURVE_WITH_KNOTS((3,3),(0.0303639456287982,0.0450225821689597),
 .UNSPECIFIED.)
CURVE()
GEOMETRIC_REPRESENTATION_ITEM()
RATIONAL_B_SPLINE_CURVE((1.00021631089164,1.00016036906093,1.))
REPRESENTATION_ITEM('')
);
#223=(
BOUNDED_CURVE()
B_SPLINE_CURVE(2,(#6635,#6636,#6637),.UNSPECIFIED.,.F.,.F.)
B_SPLINE_CURVE_WITH_KNOTS((3,3),(0.,0.0187833832018332),.UNSPECIFIED.)
CURVE()
GEOMETRIC_REPRESENTATION_ITEM()
RATIONAL_B_SPLINE_CURVE((1.,1.0014465102333,1.00204161237231))
REPRESENTATION_ITEM('')
);
#224=(
BOUNDED_CURVE()
B_SPLINE_CURVE(2,(#6641,#6642,#6643),.UNSPECIFIED.,.F.,.F.)
B_SPLINE_CURVE_WITH_KNOTS((3,3),(0.,0.0289695421536071),.UNSPECIFIED.)
CURVE()
GEOMETRIC_REPRESENTATION_ITEM()
RATIONAL_B_SPLINE_CURVE((1.,1.,1.))
REPRESENTATION_ITEM('')
);
#225=(
BOUNDED_CURVE()
B_SPLINE_CURVE(2,(#6647,#6648,#6649),.UNSPECIFIED.,.F.,.F.)
B_SPLINE_CURVE_WITH_KNOTS((3,3),(0.,0.0309504086115573),.UNSPECIFIED.)
CURVE()
GEOMETRIC_REPRESENTATION_ITEM()
RATIONAL_B_SPLINE_CURVE((1.,1.,1.))
REPRESENTATION_ITEM('')
);
#226=(
BOUNDED_CURVE()
B_SPLINE_CURVE(2,(#6653,#6654,#6655),.UNSPECIFIED.,.F.,.F.)
B_SPLINE_CURVE_WITH_KNOTS((3,3),(0.0450411357331602,0.0638245189349933),
 .UNSPECIFIED.)
CURVE()
GEOMETRIC_REPRESENTATION_ITEM()
RATIONAL_B_SPLINE_CURVE((1.00204161237231,1.0014465102333,1.))
REPRESENTATION_ITEM('')
);
#227=(
BOUNDED_CURVE()
B_SPLINE_CURVE(2,(#6662,#6663,#6664),.UNSPECIFIED.,.F.,.F.)
B_SPLINE_CURVE_WITH_KNOTS((3,3),(0.,0.0146586365398684),.UNSPECIFIED.)
CURVE()
GEOMETRIC_REPRESENTATION_ITEM()
RATIONAL_B_SPLINE_CURVE((1.,1.00016036906092,1.00021631089164))
REPRESENTATION_ITEM('')
);
#228=(
BOUNDED_CURVE()
B_SPLINE_CURVE(2,(#6668,#6669,#6670),.UNSPECIFIED.,.F.,.F.)
B_SPLINE_CURVE_WITH_KNOTS((3,3),(0.,0.0309504086115573),.UNSPECIFIED.)
CURVE()
GEOMETRIC_REPRESENTATION_ITEM()
RATIONAL_B_SPLINE_CURVE((1.,1.,1.))
REPRESENTATION_ITEM('')
);
#229=(
BOUNDED_CURVE()
B_SPLINE_CURVE(2,(#6674,#6675,#6676),.UNSPECIFIED.,.F.,.F.)
B_SPLINE_CURVE_WITH_KNOTS((3,3),(0.,0.0289695421536071),.UNSPECIFIED.)
CURVE()
GEOMETRIC_REPRESENTATION_ITEM()
RATIONAL_B_SPLINE_CURVE((1.,1.,1.))
REPRESENTATION_ITEM('')
);
#230=(
BOUNDED_CURVE()
B_SPLINE_CURVE(2,(#6680,#6681,#6682),.UNSPECIFIED.,.F.,.F.)
B_SPLINE_CURVE_WITH_KNOTS((3,3),(0.0303678686581102,0.0450284286877096),
 .UNSPECIFIED.)
CURVE()
GEOMETRIC_REPRESENTATION_ITEM()
RATIONAL_B_SPLINE_CURVE((1.00021903389143,1.00016374915722,1.00000403669809))
REPRESENTATION_ITEM('')
);
#231=(
BOUNDED_CURVE()
B_SPLINE_CURVE(2,(#6689,#6690,#6691),.UNSPECIFIED.,.F.,.F.)
B_SPLINE_CURVE_WITH_KNOTS((3,3),(0.,0.0187833832018332),.UNSPECIFIED.)
CURVE()
GEOMETRIC_REPRESENTATION_ITEM()
RATIONAL_B_SPLINE_CURVE((1.,1.0014465102333,1.00204161237231))
REPRESENTATION_ITEM('')
);
#232=(
BOUNDED_CURVE()
B_SPLINE_CURVE(2,(#6695,#6696,#6697),.UNSPECIFIED.,.F.,.F.)
B_SPLINE_CURVE_WITH_KNOTS((3,3),(0.,0.0289695421536071),.UNSPECIFIED.)
CURVE()
GEOMETRIC_REPRESENTATION_ITEM()
RATIONAL_B_SPLINE_CURVE((1.,1.,1.))
REPRESENTATION_ITEM('')
);
#233=(
BOUNDED_CURVE()
B_SPLINE_CURVE(2,(#6701,#6702,#6703),.UNSPECIFIED.,.F.,.F.)
B_SPLINE_CURVE_WITH_KNOTS((3,3),(0.,0.0309504086115573),.UNSPECIFIED.)
CURVE()
GEOMETRIC_REPRESENTATION_ITEM()
RATIONAL_B_SPLINE_CURVE((1.,1.,1.))
REPRESENTATION_ITEM('')
);
#234=(
BOUNDED_CURVE()
B_SPLINE_CURVE(2,(#6707,#6708,#6709),.UNSPECIFIED.,.F.,.F.)
B_SPLINE_CURVE_WITH_KNOTS((3,3),(0.0450411357331602,0.0638245189349933),
 .UNSPECIFIED.)
CURVE()
GEOMETRIC_REPRESENTATION_ITEM()
RATIONAL_B_SPLINE_CURVE((1.00204161237231,1.0014465102333,1.))
REPRESENTATION_ITEM('')
);
#235=(
BOUNDED_CURVE()
B_SPLINE_CURVE(2,(#6716,#6717,#6718),.UNSPECIFIED.,.F.,.F.)
B_SPLINE_CURVE_WITH_KNOTS((3,3),(0.,0.014658636844145),.UNSPECIFIED.)
CURVE()
GEOMETRIC_REPRESENTATION_ITEM()
RATIONAL_B_SPLINE_CURVE((1.,1.00016036906825,1.00021631090007))
REPRESENTATION_ITEM('')
);
#236=SHAPE_REPRESENTATION_RELATIONSHIP('SRR','None',#11479,#248);
#237=SHAPE_REPRESENTATION_RELATIONSHIP('SRR','None',#11480,#249);
#238=SHAPE_REPRESENTATION_RELATIONSHIP('SRR','None',#11481,#250);
#239=SHAPE_REPRESENTATION_RELATIONSHIP('SRR','None',#11482,#251);
#240=SHAPE_REPRESENTATION_RELATIONSHIP('SRR','None',#11483,#252);
#241=SHAPE_REPRESENTATION_RELATIONSHIP('SRR','None',#11484,#253);
#242=SHAPE_REPRESENTATION_RELATIONSHIP('SRR','None',#11485,#254);
#243=SHAPE_REPRESENTATION_RELATIONSHIP('SRR','None',#11486,#255);
#244=SHAPE_REPRESENTATION_RELATIONSHIP('SRR','None',#11487,#256);
#245=SHAPE_REPRESENTATION_RELATIONSHIP('SRR','None',#11488,#257);
#246=SHAPE_REPRESENTATION_RELATIONSHIP('SRR','None',#11489,#258);
#247=SHAPE_REPRESENTATION_RELATIONSHIP('SRR','None',#11490,#259);
#248=ADVANCED_BREP_SHAPE_REPRESENTATION('',(#272),#11418);
#249=ADVANCED_BREP_SHAPE_REPRESENTATION('',(#273),#11419);
#250=ADVANCED_BREP_SHAPE_REPRESENTATION('',(#274),#11420);
#251=ADVANCED_BREP_SHAPE_REPRESENTATION('',(#275),#11421);
#252=ADVANCED_BREP_SHAPE_REPRESENTATION('',(#276),#11422);
#253=ADVANCED_BREP_SHAPE_REPRESENTATION('',(#277),#11423);
#254=ADVANCED_BREP_SHAPE_REPRESENTATION('',(#278),#11424);
#255=ADVANCED_BREP_SHAPE_REPRESENTATION('',(#279),#11425);
#256=ADVANCED_BREP_SHAPE_REPRESENTATION('',(#280),#11426);
#257=ADVANCED_BREP_SHAPE_REPRESENTATION('',(#281),#11427);
#258=ADVANCED_BREP_SHAPE_REPRESENTATION('',(#282),#11428);
#259=ADVANCED_BREP_SHAPE_REPRESENTATION('',(#283),#11429);
#260=STYLED_ITEM('',(#11588),#272);
#261=STYLED_ITEM('',(#11602),#273);
#262=STYLED_ITEM('',(#11609),#274);
#263=STYLED_ITEM('',(#11616),#275);
#264=STYLED_ITEM('',(#11623),#276);
#265=STYLED_ITEM('',(#11616),#277);
#266=STYLED_ITEM('',(#11616),#278);
#267=STYLED_ITEM('',(#11609),#279);
#268=STYLED_ITEM('',(#11623),#280);
#269=STYLED_ITEM('',(#11623),#281);
#270=STYLED_ITEM('',(#11616),#282);
#271=STYLED_ITEM('',(#11623),#283);
#272=MANIFOLD_SOLID_BREP('Body1',#4461);
#273=MANIFOLD_SOLID_BREP('Body1',#4462);
#274=MANIFOLD_SOLID_BREP('Body1',#4463);
#275=MANIFOLD_SOLID_BREP('Body1',#4464);
#276=MANIFOLD_SOLID_BREP('Body1',#4465);
#277=MANIFOLD_SOLID_BREP('Body1',#4466);
#278=MANIFOLD_SOLID_BREP('Body1',#4467);
#279=MANIFOLD_SOLID_BREP('Body1',#4468);
#280=MANIFOLD_SOLID_BREP('Body1',#4469);
#281=MANIFOLD_SOLID_BREP('Body1',#4470);
#282=MANIFOLD_SOLID_BREP('Body1',#4471);
#283=MANIFOLD_SOLID_BREP('Body1',#4472);
#284=FACE_BOUND('',#797,.T.);
#285=FACE_BOUND('',#800,.T.);
#286=FACE_BOUND('',#804,.T.);
#287=FACE_BOUND('',#833,.T.);
#288=FACE_BOUND('',#836,.T.);
#289=FACE_BOUND('',#842,.T.);
#290=FACE_BOUND('',#847,.T.);
#291=FACE_BOUND('',#851,.T.);
#292=FACE_BOUND('',#854,.T.);
#293=FACE_BOUND('',#857,.T.);
#294=FACE_BOUND('',#862,.T.);
#295=FACE_BOUND('',#865,.T.);
#296=FACE_BOUND('',#868,.T.);
#297=FACE_BOUND('',#873,.T.);
#298=FACE_BOUND('',#876,.T.);
#299=FACE_BOUND('',#879,.T.);
#300=FACE_BOUND('',#901,.T.);
#301=FACE_BOUND('',#902,.T.);
#302=FACE_BOUND('',#903,.T.);
#303=FACE_BOUND('',#912,.T.);
#304=FACE_BOUND('',#913,.T.);
#305=FACE_BOUND('',#914,.T.);
#306=FACE_BOUND('',#944,.T.);
#307=FACE_BOUND('',#966,.T.);
#308=FACE_BOUND('',#976,.T.);
#309=FACE_BOUND('',#981,.T.);
#310=FACE_BOUND('',#992,.T.);
#311=FACE_BOUND('',#993,.T.);
#312=FACE_BOUND('',#1015,.T.);
#313=FACE_BOUND('',#1022,.T.);
#314=FACE_BOUND('',#1029,.T.);
#315=FACE_BOUND('',#1031,.T.);
#316=FACE_BOUND('',#1034,.T.);
#317=FACE_BOUND('',#1037,.T.);
#318=FACE_BOUND('',#1040,.T.);
#319=FACE_BOUND('',#1077,.T.);
#320=FACE_BOUND('',#1088,.T.);
#321=FACE_BOUND('',#1094,.T.);
#322=FACE_BOUND('',#1097,.T.);
#323=PLANE('',#4614);
#324=PLANE('',#4619);
#325=PLANE('',#4629);
#326=PLANE('',#4636);
#327=PLANE('',#4639);
#328=PLANE('',#4642);
#329=PLANE('',#4645);
#330=PLANE('',#4650);
#331=PLANE('',#4653);
#332=PLANE('',#4654);
#333=PLANE('',#4657);
#334=PLANE('',#4660);
#335=PLANE('',#4662);
#336=PLANE('',#4665);
#337=PLANE('',#4667);
#338=PLANE('',#4670);
#339=PLANE('',#4671);
#340=PLANE('',#4675);
#341=PLANE('',#4676);
#342=PLANE('',#4685);
#343=PLANE('',#4693);
#344=PLANE('',#4699);
#345=PLANE('',#4704);
#346=PLANE('',#4708);
#347=PLANE('',#4716);
#348=PLANE('',#4720);
#349=PLANE('',#4724);
#350=PLANE('',#4732);
#351=PLANE('',#4737);
#352=PLANE('',#4741);
#353=PLANE('',#4743);
#354=PLANE('',#4744);
#355=PLANE('',#4745);
#356=PLANE('',#4746);
#357=PLANE('',#4747);
#358=PLANE('',#4748);
#359=PLANE('',#4749);
#360=PLANE('',#4750);
#361=PLANE('',#4751);
#362=PLANE('',#4758);
#363=PLANE('',#4759);
#364=PLANE('',#4764);
#365=PLANE('',#4776);
#366=PLANE('',#4798);
#367=PLANE('',#4801);
#368=PLANE('',#4802);
#369=PLANE('',#4820);
#370=PLANE('',#4823);
#371=PLANE('',#4828);
#372=PLANE('',#4829);
#373=PLANE('',#4830);
#374=PLANE('',#4831);
#375=PLANE('',#4832);
#376=PLANE('',#4833);
#377=PLANE('',#4834);
#378=PLANE('',#4835);
#379=PLANE('',#4842);
#380=PLANE('',#4856);
#381=PLANE('',#4861);
#382=PLANE('',#4862);
#383=PLANE('',#4863);
#384=PLANE('',#4869);
#385=PLANE('',#4871);
#386=PLANE('',#4873);
#387=PLANE('',#4875);
#388=PLANE('',#4877);
#389=PLANE('',#4879);
#390=PLANE('',#4881);
#391=PLANE('',#4888);
#392=PLANE('',#4893);
#393=PLANE('',#4904);
#394=PLANE('',#4909);
#395=PLANE('',#4915);
#396=PLANE('',#4919);
#397=PLANE('',#4923);
#398=PLANE('',#4927);
#399=PLANE('',#4937);
#400=PLANE('',#4941);
#401=PLANE('',#4945);
#402=PLANE('',#4949);
#403=PLANE('',#4959);
#404=PLANE('',#4965);
#405=PLANE('',#4966);
#406=PLANE('',#4969);
#407=PLANE('',#4975);
#408=PLANE('',#4976);
#409=PLANE('',#4981);
#410=PLANE('',#4985);
#411=PLANE('',#4989);
#412=PLANE('',#5017);
#413=PLANE('',#5022);
#414=PLANE('',#5023);
#415=PLANE('',#5024);
#416=PLANE('',#5025);
#417=PLANE('',#5026);
#418=PLANE('',#5027);
#419=PLANE('',#5028);
#420=PLANE('',#5029);
#421=PLANE('',#5031);
#422=PLANE('',#5032);
#423=PLANE('',#5033);
#424=PLANE('',#5034);
#425=PLANE('',#5035);
#426=PLANE('',#5036);
#427=PLANE('',#5037);
#428=PLANE('',#5042);
#429=PLANE('',#5055);
#430=PLANE('',#5059);
#431=CYLINDRICAL_SURFACE('',#4611,3.);
#432=CYLINDRICAL_SURFACE('',#4624,5.005);
#433=CYLINDRICAL_SURFACE('',#4634,5.005);
#434=CYLINDRICAL_SURFACE('',#4648,4.);
#435=CYLINDRICAL_SURFACE('',#4651,4.);
#436=CYLINDRICAL_SURFACE('',#4664,4.);
#437=CYLINDRICAL_SURFACE('',#4666,4.);
#438=CYLINDRICAL_SURFACE('',#4668,1.3);
#439=CYLINDRICAL_SURFACE('',#4673,4.25);
#440=CYLINDRICAL_SURFACE('',#4684,2.515);
#441=CYLINDRICAL_SURFACE('',#4689,4.);
#442=CYLINDRICAL_SURFACE('',#4695,3.);
#443=CYLINDRICAL_SURFACE('',#4712,5.);
#444=CYLINDRICAL_SURFACE('',#4728,3.);
#445=CYLINDRICAL_SURFACE('',#4734,3.05);
#446=CYLINDRICAL_SURFACE('',#4739,4.);
#447=CYLINDRICAL_SURFACE('',#4768,3.);
#448=CYLINDRICAL_SURFACE('',#4770,5.5);
#449=CYLINDRICAL_SURFACE('',#4772,5.5);
#450=CYLINDRICAL_SURFACE('',#4774,3.);
#451=CYLINDRICAL_SURFACE('',#4785,5.5);
#452=CYLINDRICAL_SURFACE('',#4786,1.05);
#453=CYLINDRICAL_SURFACE('',#4803,1.52);
#454=CYLINDRICAL_SURFACE('',#4804,1.52);
#455=CYLINDRICAL_SURFACE('',#4805,3.01);
#456=CYLINDRICAL_SURFACE('',#4807,0.96675);
#457=CYLINDRICAL_SURFACE('',#4809,0.96675);
#458=CYLINDRICAL_SURFACE('',#4810,0.96675);
#459=CYLINDRICAL_SURFACE('',#4811,0.96675);
#460=CYLINDRICAL_SURFACE('',#4812,0.96675);
#461=CYLINDRICAL_SURFACE('',#4813,0.96675);
#462=CYLINDRICAL_SURFACE('',#4814,0.739);
#463=CYLINDRICAL_SURFACE('',#4816,0.739);
#464=CYLINDRICAL_SURFACE('',#4817,0.739);
#465=CYLINDRICAL_SURFACE('',#4818,0.739);
#466=CYLINDRICAL_SURFACE('',#4819,0.739);
#467=CYLINDRICAL_SURFACE('',#4827,0.739);
#468=CYLINDRICAL_SURFACE('',#4838,0.96675);
#469=CYLINDRICAL_SURFACE('',#4844,1.215);
#470=CYLINDRICAL_SURFACE('',#4846,1.215);
#471=CYLINDRICAL_SURFACE('',#4847,1.215);
#472=CYLINDRICAL_SURFACE('',#4848,1.215);
#473=CYLINDRICAL_SURFACE('',#4849,1.215);
#474=CYLINDRICAL_SURFACE('',#4850,0.95825);
#475=CYLINDRICAL_SURFACE('',#4852,0.95825);
#476=CYLINDRICAL_SURFACE('',#4853,0.95825);
#477=CYLINDRICAL_SURFACE('',#4854,0.95825);
#478=CYLINDRICAL_SURFACE('',#4855,0.95825);
#479=CYLINDRICAL_SURFACE('',#4860,0.95825);
#480=CYLINDRICAL_SURFACE('',#4867,2.25);
#481=CYLINDRICAL_SURFACE('',#4891,1.215);
#482=CYLINDRICAL_SURFACE('',#4895,2.25);
#483=CYLINDRICAL_SURFACE('',#4896,1.5);
#484=CYLINDRICAL_SURFACE('',#4912,0.800000000000001);
#485=CYLINDRICAL_SURFACE('',#4913,2.5);
#486=CYLINDRICAL_SURFACE('',#4961,0.8);
#487=CYLINDRICAL_SURFACE('',#4962,3.8);
#488=CYLINDRICAL_SURFACE('',#4963,0.8);
#489=CYLINDRICAL_SURFACE('',#4964,0.8);
#490=CYLINDRICAL_SURFACE('',#4968,3.);
#491=CYLINDRICAL_SURFACE('',#4970,0.8);
#492=CYLINDRICAL_SURFACE('',#4971,2.01);
#493=CYLINDRICAL_SURFACE('',#4973,1.05);
#494=CYLINDRICAL_SURFACE('',#4978,1.05);
#495=CYLINDRICAL_SURFACE('',#4983,1.5);
#496=CYLINDRICAL_SURFACE('',#4987,2.25);
#497=CYLINDRICAL_SURFACE('',#4991,0.96675);
#498=CYLINDRICAL_SURFACE('',#4993,0.96675);
#499=CYLINDRICAL_SURFACE('',#4994,0.96675);
#500=CYLINDRICAL_SURFACE('',#4995,0.96675);
#501=CYLINDRICAL_SURFACE('',#4996,0.96675);
#502=CYLINDRICAL_SURFACE('',#4997,0.96675);
#503=CYLINDRICAL_SURFACE('',#4998,0.96675);
#504=CYLINDRICAL_SURFACE('',#4999,0.96675);
#505=CYLINDRICAL_SURFACE('',#5000,0.96675);
#506=CYLINDRICAL_SURFACE('',#5001,0.96675);
#507=CYLINDRICAL_SURFACE('',#5002,0.96675);
#508=CYLINDRICAL_SURFACE('',#5003,0.96675);
#509=CYLINDRICAL_SURFACE('',#5004,0.739);
#510=CYLINDRICAL_SURFACE('',#5006,0.739);
#511=CYLINDRICAL_SURFACE('',#5007,0.739);
#512=CYLINDRICAL_SURFACE('',#5008,0.739);
#513=CYLINDRICAL_SURFACE('',#5009,0.739);
#514=CYLINDRICAL_SURFACE('',#5010,0.739);
#515=CYLINDRICAL_SURFACE('',#5011,0.739);
#516=CYLINDRICAL_SURFACE('',#5012,0.739);
#517=CYLINDRICAL_SURFACE('',#5013,0.739);
#518=CYLINDRICAL_SURFACE('',#5014,0.739);
#519=CYLINDRICAL_SURFACE('',#5015,0.739);
#520=CYLINDRICAL_SURFACE('',#5016,0.739);
#521=CYLINDRICAL_SURFACE('',#5021,0.739);
#522=CYLINDRICAL_SURFACE('',#5040,0.96675);
#523=CYLINDRICAL_SURFACE('',#5044,2.);
#524=CYLINDRICAL_SURFACE('',#5052,1.25);
#525=CYLINDRICAL_SURFACE('',#5063,2.);
#526=FACE_OUTER_BOUND('',#794,.T.);
#527=FACE_OUTER_BOUND('',#795,.T.);
#528=FACE_OUTER_BOUND('',#796,.T.);
#529=FACE_OUTER_BOUND('',#798,.T.);
#530=FACE_OUTER_BOUND('',#799,.T.);
#531=FACE_OUTER_BOUND('',#801,.T.);
#532=FACE_OUTER_BOUND('',#802,.T.);
#533=FACE_OUTER_BOUND('',#803,.T.);
#534=FACE_OUTER_BOUND('',#805,.T.);
#535=FACE_OUTER_BOUND('',#806,.T.);
#536=FACE_OUTER_BOUND('',#807,.T.);
#537=FACE_OUTER_BOUND('',#808,.T.);
#538=FACE_OUTER_BOUND('',#809,.T.);
#539=FACE_OUTER_BOUND('',#810,.T.);
#540=FACE_OUTER_BOUND('',#811,.T.);
#541=FACE_OUTER_BOUND('',#812,.T.);
#542=FACE_OUTER_BOUND('',#813,.T.);
#543=FACE_OUTER_BOUND('',#814,.T.);
#544=FACE_OUTER_BOUND('',#815,.T.);
#545=FACE_OUTER_BOUND('',#816,.T.);
#546=FACE_OUTER_BOUND('',#817,.T.);
#547=FACE_OUTER_BOUND('',#818,.T.);
#548=FACE_OUTER_BOUND('',#819,.T.);
#549=FACE_OUTER_BOUND('',#820,.T.);
#550=FACE_OUTER_BOUND('',#821,.T.);
#551=FACE_OUTER_BOUND('',#822,.T.);
#552=FACE_OUTER_BOUND('',#823,.T.);
#553=FACE_OUTER_BOUND('',#824,.T.);
#554=FACE_OUTER_BOUND('',#825,.T.);
#555=FACE_OUTER_BOUND('',#826,.T.);
#556=FACE_OUTER_BOUND('',#827,.T.);
#557=FACE_OUTER_BOUND('',#828,.T.);
#558=FACE_OUTER_BOUND('',#829,.T.);
#559=FACE_OUTER_BOUND('',#830,.T.);
#560=FACE_OUTER_BOUND('',#831,.T.);
#561=FACE_OUTER_BOUND('',#832,.T.);
#562=FACE_OUTER_BOUND('',#834,.T.);
#563=FACE_OUTER_BOUND('',#835,.T.);
#564=FACE_OUTER_BOUND('',#837,.T.);
#565=FACE_OUTER_BOUND('',#838,.T.);
#566=FACE_OUTER_BOUND('',#839,.T.);
#567=FACE_OUTER_BOUND('',#840,.T.);
#568=FACE_OUTER_BOUND('',#841,.T.);
#569=FACE_OUTER_BOUND('',#843,.T.);
#570=FACE_OUTER_BOUND('',#844,.T.);
#571=FACE_OUTER_BOUND('',#845,.T.);
#572=FACE_OUTER_BOUND('',#846,.T.);
#573=FACE_OUTER_BOUND('',#848,.T.);
#574=FACE_OUTER_BOUND('',#849,.T.);
#575=FACE_OUTER_BOUND('',#850,.T.);
#576=FACE_OUTER_BOUND('',#852,.T.);
#577=FACE_OUTER_BOUND('',#853,.T.);
#578=FACE_OUTER_BOUND('',#855,.T.);
#579=FACE_OUTER_BOUND('',#856,.T.);
#580=FACE_OUTER_BOUND('',#858,.T.);
#581=FACE_OUTER_BOUND('',#859,.T.);
#582=FACE_OUTER_BOUND('',#860,.T.);
#583=FACE_OUTER_BOUND('',#861,.T.);
#584=FACE_OUTER_BOUND('',#863,.T.);
#585=FACE_OUTER_BOUND('',#864,.T.);
#586=FACE_OUTER_BOUND('',#866,.T.);
#587=FACE_OUTER_BOUND('',#867,.T.);
#588=FACE_OUTER_BOUND('',#869,.T.);
#589=FACE_OUTER_BOUND('',#870,.T.);
#590=FACE_OUTER_BOUND('',#871,.T.);
#591=FACE_OUTER_BOUND('',#872,.T.);
#592=FACE_OUTER_BOUND('',#874,.T.);
#593=FACE_OUTER_BOUND('',#875,.T.);
#594=FACE_OUTER_BOUND('',#877,.T.);
#595=FACE_OUTER_BOUND('',#878,.T.);
#596=FACE_OUTER_BOUND('',#880,.T.);
#597=FACE_OUTER_BOUND('',#881,.T.);
#598=FACE_OUTER_BOUND('',#882,.T.);
#599=FACE_OUTER_BOUND('',#883,.T.);
#600=FACE_OUTER_BOUND('',#884,.T.);
#601=FACE_OUTER_BOUND('',#885,.T.);
#602=FACE_OUTER_BOUND('',#886,.T.);
#603=FACE_OUTER_BOUND('',#887,.T.);
#604=FACE_OUTER_BOUND('',#888,.T.);
#605=FACE_OUTER_BOUND('',#889,.T.);
#606=FACE_OUTER_BOUND('',#890,.T.);
#607=FACE_OUTER_BOUND('',#891,.T.);
#608=FACE_OUTER_BOUND('',#892,.T.);
#609=FACE_OUTER_BOUND('',#893,.T.);
#610=FACE_OUTER_BOUND('',#894,.T.);
#611=FACE_OUTER_BOUND('',#895,.T.);
#612=FACE_OUTER_BOUND('',#896,.T.);
#613=FACE_OUTER_BOUND('',#897,.T.);
#614=FACE_OUTER_BOUND('',#898,.T.);
#615=FACE_OUTER_BOUND('',#899,.T.);
#616=FACE_OUTER_BOUND('',#900,.T.);
#617=FACE_OUTER_BOUND('',#904,.T.);
#618=FACE_OUTER_BOUND('',#905,.T.);
#619=FACE_OUTER_BOUND('',#906,.T.);
#620=FACE_OUTER_BOUND('',#907,.T.);
#621=FACE_OUTER_BOUND('',#908,.T.);
#622=FACE_OUTER_BOUND('',#909,.T.);
#623=FACE_OUTER_BOUND('',#910,.T.);
#624=FACE_OUTER_BOUND('',#911,.T.);
#625=FACE_OUTER_BOUND('',#915,.T.);
#626=FACE_OUTER_BOUND('',#916,.T.);
#627=FACE_OUTER_BOUND('',#917,.T.);
#628=FACE_OUTER_BOUND('',#918,.T.);
#629=FACE_OUTER_BOUND('',#919,.T.);
#630=FACE_OUTER_BOUND('',#920,.T.);
#631=FACE_OUTER_BOUND('',#921,.T.);
#632=FACE_OUTER_BOUND('',#922,.T.);
#633=FACE_OUTER_BOUND('',#923,.T.);
#634=FACE_OUTER_BOUND('',#924,.T.);
#635=FACE_OUTER_BOUND('',#925,.T.);
#636=FACE_OUTER_BOUND('',#926,.T.);
#637=FACE_OUTER_BOUND('',#927,.T.);
#638=FACE_OUTER_BOUND('',#928,.T.);
#639=FACE_OUTER_BOUND('',#929,.T.);
#640=FACE_OUTER_BOUND('',#930,.T.);
#641=FACE_OUTER_BOUND('',#931,.T.);
#642=FACE_OUTER_BOUND('',#932,.T.);
#643=FACE_OUTER_BOUND('',#933,.T.);
#644=FACE_OUTER_BOUND('',#934,.T.);
#645=FACE_OUTER_BOUND('',#935,.T.);
#646=FACE_OUTER_BOUND('',#936,.T.);
#647=FACE_OUTER_BOUND('',#937,.T.);
#648=FACE_OUTER_BOUND('',#938,.T.);
#649=FACE_OUTER_BOUND('',#939,.T.);
#650=FACE_OUTER_BOUND('',#940,.T.);
#651=FACE_OUTER_BOUND('',#941,.T.);
#652=FACE_OUTER_BOUND('',#942,.T.);
#653=FACE_OUTER_BOUND('',#943,.T.);
#654=FACE_OUTER_BOUND('',#945,.T.);
#655=FACE_OUTER_BOUND('',#946,.T.);
#656=FACE_OUTER_BOUND('',#947,.T.);
#657=FACE_OUTER_BOUND('',#948,.T.);
#658=FACE_OUTER_BOUND('',#949,.T.);
#659=FACE_OUTER_BOUND('',#950,.T.);
#660=FACE_OUTER_BOUND('',#951,.T.);
#661=FACE_OUTER_BOUND('',#952,.T.);
#662=FACE_OUTER_BOUND('',#953,.T.);
#663=FACE_OUTER_BOUND('',#954,.T.);
#664=FACE_OUTER_BOUND('',#955,.T.);
#665=FACE_OUTER_BOUND('',#956,.T.);
#666=FACE_OUTER_BOUND('',#957,.T.);
#667=FACE_OUTER_BOUND('',#958,.T.);
#668=FACE_OUTER_BOUND('',#959,.T.);
#669=FACE_OUTER_BOUND('',#960,.T.);
#670=FACE_OUTER_BOUND('',#961,.T.);
#671=FACE_OUTER_BOUND('',#962,.T.);
#672=FACE_OUTER_BOUND('',#963,.T.);
#673=FACE_OUTER_BOUND('',#964,.T.);
#674=FACE_OUTER_BOUND('',#965,.T.);
#675=FACE_OUTER_BOUND('',#967,.T.);
#676=FACE_OUTER_BOUND('',#968,.T.);
#677=FACE_OUTER_BOUND('',#969,.T.);
#678=FACE_OUTER_BOUND('',#970,.T.);
#679=FACE_OUTER_BOUND('',#971,.T.);
#680=FACE_OUTER_BOUND('',#972,.T.);
#681=FACE_OUTER_BOUND('',#973,.T.);
#682=FACE_OUTER_BOUND('',#974,.T.);
#683=FACE_OUTER_BOUND('',#975,.T.);
#684=FACE_OUTER_BOUND('',#977,.T.);
#685=FACE_OUTER_BOUND('',#978,.T.);
#686=FACE_OUTER_BOUND('',#979,.T.);
#687=FACE_OUTER_BOUND('',#980,.T.);
#688=FACE_OUTER_BOUND('',#982,.T.);
#689=FACE_OUTER_BOUND('',#983,.T.);
#690=FACE_OUTER_BOUND('',#984,.T.);
#691=FACE_OUTER_BOUND('',#985,.T.);
#692=FACE_OUTER_BOUND('',#986,.T.);
#693=FACE_OUTER_BOUND('',#987,.T.);
#694=FACE_OUTER_BOUND('',#988,.T.);
#695=FACE_OUTER_BOUND('',#989,.T.);
#696=FACE_OUTER_BOUND('',#990,.T.);
#697=FACE_OUTER_BOUND('',#991,.T.);
#698=FACE_OUTER_BOUND('',#994,.T.);
#699=FACE_OUTER_BOUND('',#995,.T.);
#700=FACE_OUTER_BOUND('',#996,.T.);
#701=FACE_OUTER_BOUND('',#997,.T.);
#702=FACE_OUTER_BOUND('',#998,.T.);
#703=FACE_OUTER_BOUND('',#999,.T.);
#704=FACE_OUTER_BOUND('',#1000,.T.);
#705=FACE_OUTER_BOUND('',#1001,.T.);
#706=FACE_OUTER_BOUND('',#1002,.T.);
#707=FACE_OUTER_BOUND('',#1003,.T.);
#708=FACE_OUTER_BOUND('',#1004,.T.);
#709=FACE_OUTER_BOUND('',#1005,.T.);
#710=FACE_OUTER_BOUND('',#1006,.T.);
#711=FACE_OUTER_BOUND('',#1007,.T.);
#712=FACE_OUTER_BOUND('',#1008,.T.);
#713=FACE_OUTER_BOUND('',#1009,.T.);
#714=FACE_OUTER_BOUND('',#1010,.T.);
#715=FACE_OUTER_BOUND('',#1011,.T.);
#716=FACE_OUTER_BOUND('',#1012,.T.);
#717=FACE_OUTER_BOUND('',#1013,.T.);
#718=FACE_OUTER_BOUND('',#1014,.T.);
#719=FACE_OUTER_BOUND('',#1016,.T.);
#720=FACE_OUTER_BOUND('',#1017,.T.);
#721=FACE_OUTER_BOUND('',#1018,.T.);
#722=FACE_OUTER_BOUND('',#1019,.T.);
#723=FACE_OUTER_BOUND('',#1020,.T.);
#724=FACE_OUTER_BOUND('',#1021,.T.);
#725=FACE_OUTER_BOUND('',#1023,.T.);
#726=FACE_OUTER_BOUND('',#1024,.T.);
#727=FACE_OUTER_BOUND('',#1025,.T.);
#728=FACE_OUTER_BOUND('',#1026,.T.);
#729=FACE_OUTER_BOUND('',#1027,.T.);
#730=FACE_OUTER_BOUND('',#1028,.T.);
#731=FACE_OUTER_BOUND('',#1030,.T.);
#732=FACE_OUTER_BOUND('',#1032,.T.);
#733=FACE_OUTER_BOUND('',#1033,.T.);
#734=FACE_OUTER_BOUND('',#1035,.T.);
#735=FACE_OUTER_BOUND('',#1036,.T.);
#736=FACE_OUTER_BOUND('',#1038,.T.);
#737=FACE_OUTER_BOUND('',#1039,.T.);
#738=FACE_OUTER_BOUND('',#1041,.T.);
#739=FACE_OUTER_BOUND('',#1042,.T.);
#740=FACE_OUTER_BOUND('',#1043,.T.);
#741=FACE_OUTER_BOUND('',#1044,.T.);
#742=FACE_OUTER_BOUND('',#1045,.T.);
#743=FACE_OUTER_BOUND('',#1046,.T.);
#744=FACE_OUTER_BOUND('',#1047,.T.);
#745=FACE_OUTER_BOUND('',#1048,.T.);
#746=FACE_OUTER_BOUND('',#1049,.T.);
#747=FACE_OUTER_BOUND('',#1050,.T.);
#748=FACE_OUTER_BOUND('',#1051,.T.);
#749=FACE_OUTER_BOUND('',#1052,.T.);
#750=FACE_OUTER_BOUND('',#1053,.T.);
#751=FACE_OUTER_BOUND('',#1054,.T.);
#752=FACE_OUTER_BOUND('',#1055,.T.);
#753=FACE_OUTER_BOUND('',#1056,.T.);
#754=FACE_OUTER_BOUND('',#1057,.T.);
#755=FACE_OUTER_BOUND('',#1058,.T.);
#756=FACE_OUTER_BOUND('',#1059,.T.);
#757=FACE_OUTER_BOUND('',#1060,.T.);
#758=FACE_OUTER_BOUND('',#1061,.T.);
#759=FACE_OUTER_BOUND('',#1062,.T.);
#760=FACE_OUTER_BOUND('',#1063,.T.);
#761=FACE_OUTER_BOUND('',#1064,.T.);
#762=FACE_OUTER_BOUND('',#1065,.T.);
#763=FACE_OUTER_BOUND('',#1066,.T.);
#764=FACE_OUTER_BOUND('',#1067,.T.);
#765=FACE_OUTER_BOUND('',#1068,.T.);
#766=FACE_OUTER_BOUND('',#1069,.T.);
#767=FACE_OUTER_BOUND('',#1070,.T.);
#768=FACE_OUTER_BOUND('',#1071,.T.);
#769=FACE_OUTER_BOUND('',#1072,.T.);
#770=FACE_OUTER_BOUND('',#1073,.T.);
#771=FACE_OUTER_BOUND('',#1074,.T.);
#772=FACE_OUTER_BOUND('',#1075,.T.);
#773=FACE_OUTER_BOUND('',#1076,.T.);
#774=FACE_OUTER_BOUND('',#1078,.T.);
#775=FACE_OUTER_BOUND('',#1079,.T.);
#776=FACE_OUTER_BOUND('',#1080,.T.);
#777=FACE_OUTER_BOUND('',#1081,.T.);
#778=FACE_OUTER_BOUND('',#1082,.T.);
#779=FACE_OUTER_BOUND('',#1083,.T.);
#780=FACE_OUTER_BOUND('',#1084,.T.);
#781=FACE_OUTER_BOUND('',#1085,.T.);
#782=FACE_OUTER_BOUND('',#1086,.T.);
#783=FACE_OUTER_BOUND('',#1087,.T.);
#784=FACE_OUTER_BOUND('',#1089,.T.);
#785=FACE_OUTER_BOUND('',#1090,.T.);
#786=FACE_OUTER_BOUND('',#1091,.T.);
#787=FACE_OUTER_BOUND('',#1092,.T.);
#788=FACE_OUTER_BOUND('',#1093,.T.);
#789=FACE_OUTER_BOUND('',#1095,.T.);
#790=FACE_OUTER_BOUND('',#1096,.T.);
#791=FACE_OUTER_BOUND('',#1098,.T.);
#792=FACE_OUTER_BOUND('',#1099,.T.);
#793=FACE_OUTER_BOUND('',#1100,.T.);
#794=EDGE_LOOP('',(#2885,#2886,#2887,#2888));
#795=EDGE_LOOP('',(#2889,#2890,#2891,#2892,#2893));
#796=EDGE_LOOP('',(#2894));
#797=EDGE_LOOP('',(#2895));
#798=EDGE_LOOP('',(#2896,#2897,#2898,#2899));
#799=EDGE_LOOP('',(#2900,#2901,#2902,#2903,#2904,#2905,#2906,#2907));
#800=EDGE_LOOP('',(#2908));
#801=EDGE_LOOP('',(#2909,#2910,#2911,#2912));
#802=EDGE_LOOP('',(#2913,#2914,#2915,#2916));
#803=EDGE_LOOP('',(#2917,#2918,#2919,#2920,#2921,#2922,#2923,#2924));
#804=EDGE_LOOP('',(#2925));
#805=EDGE_LOOP('',(#2926,#2927,#2928,#2929));
#806=EDGE_LOOP('',(#2930,#2931,#2932,#2933));
#807=EDGE_LOOP('',(#2934,#2935,#2936,#2937));
#808=EDGE_LOOP('',(#2938,#2939,#2940,#2941));
#809=EDGE_LOOP('',(#2942,#2943,#2944,#2945));
#810=EDGE_LOOP('',(#2946,#2947,#2948,#2949));
#811=EDGE_LOOP('',(#2950,#2951,#2952,#2953));
#812=EDGE_LOOP('',(#2954,#2955,#2956,#2957));
#813=EDGE_LOOP('',(#2958,#2959,#2960,#2961));
#814=EDGE_LOOP('',(#2962,#2963,#2964,#2965));
#815=EDGE_LOOP('',(#2966,#2967,#2968,#2969));
#816=EDGE_LOOP('',(#2970,#2971,#2972,#2973,#2974));
#817=EDGE_LOOP('',(#2975,#2976,#2977,#2978));
#818=EDGE_LOOP('',(#2979,#2980,#2981,#2982));
#819=EDGE_LOOP('',(#2983,#2984,#2985,#2986));
#820=EDGE_LOOP('',(#2987,#2988,#2989,#2990));
#821=EDGE_LOOP('',(#2991,#2992,#2993,#2994));
#822=EDGE_LOOP('',(#2995,#2996,#2997,#2998));
#823=EDGE_LOOP('',(#2999,#3000,#3001,#3002));
#824=EDGE_LOOP('',(#3003,#3004,#3005,#3006));
#825=EDGE_LOOP('',(#3007,#3008,#3009,#3010));
#826=EDGE_LOOP('',(#3011,#3012,#3013,#3014));
#827=EDGE_LOOP('',(#3015,#3016,#3017,#3018));
#828=EDGE_LOOP('',(#3019,#3020,#3021,#3022,#3023));
#829=EDGE_LOOP('',(#3024,#3025,#3026,#3027));
#830=EDGE_LOOP('',(#3028,#3029,#3030,#3031));
#831=EDGE_LOOP('',(#3032));
#832=EDGE_LOOP('',(#3033));
#833=EDGE_LOOP('',(#3034));
#834=EDGE_LOOP('',(#3035,#3036,#3037,#3038));
#835=EDGE_LOOP('',(#3039));
#836=EDGE_LOOP('',(#3040));
#837=EDGE_LOOP('',(#3041,#3042,#3043,#3044));
#838=EDGE_LOOP('',(#3045,#3046,#3047,#3048));
#839=EDGE_LOOP('',(#3049,#3050,#3051,#3052));
#840=EDGE_LOOP('',(#3053,#3054,#3055,#3056));
#841=EDGE_LOOP('',(#3057));
#842=EDGE_LOOP('',(#3058));
#843=EDGE_LOOP('',(#3059,#3060,#3061,#3062));
#844=EDGE_LOOP('',(#3063,#3064,#3065,#3066));
#845=EDGE_LOOP('',(#3067,#3068,#3069,#3070));
#846=EDGE_LOOP('',(#3071));
#847=EDGE_LOOP('',(#3072));
#848=EDGE_LOOP('',(#3073,#3074,#3075,#3076));
#849=EDGE_LOOP('',(#3077,#3078,#3079,#3080));
#850=EDGE_LOOP('',(#3081));
#851=EDGE_LOOP('',(#3082));
#852=EDGE_LOOP('',(#3083,#3084,#3085,#3086));
#853=EDGE_LOOP('',(#3087));
#854=EDGE_LOOP('',(#3088));
#855=EDGE_LOOP('',(#3089,#3090,#3091,#3092));
#856=EDGE_LOOP('',(#3093));
#857=EDGE_LOOP('',(#3094));
#858=EDGE_LOOP('',(#3095,#3096,#3097,#3098));
#859=EDGE_LOOP('',(#3099,#3100,#3101,#3102));
#860=EDGE_LOOP('',(#3103,#3104,#3105,#3106));
#861=EDGE_LOOP('',(#3107));
#862=EDGE_LOOP('',(#3108));
#863=EDGE_LOOP('',(#3109,#3110,#3111,#3112));
#864=EDGE_LOOP('',(#3113));
#865=EDGE_LOOP('',(#3114));
#866=EDGE_LOOP('',(#3115,#3116,#3117,#3118));
#867=EDGE_LOOP('',(#3119));
#868=EDGE_LOOP('',(#3120));
#869=EDGE_LOOP('',(#3121,#3122,#3123,#3124));
#870=EDGE_LOOP('',(#3125,#3126,#3127,#3128));
#871=EDGE_LOOP('',(#3129,#3130,#3131,#3132));
#872=EDGE_LOOP('',(#3133));
#873=EDGE_LOOP('',(#3134));
#874=EDGE_LOOP('',(#3135,#3136,#3137,#3138));
#875=EDGE_LOOP('',(#3139));
#876=EDGE_LOOP('',(#3140));
#877=EDGE_LOOP('',(#3141,#3142,#3143,#3144));
#878=EDGE_LOOP('',(#3145));
#879=EDGE_LOOP('',(#3146));
#880=EDGE_LOOP('',(#3147,#3148,#3149,#3150));
#881=EDGE_LOOP('',(#3151,#3152,#3153,#3154,#3155,#3156));
#882=EDGE_LOOP('',(#3157,#3158,#3159,#3160));
#883=EDGE_LOOP('',(#3161,#3162,#3163,#3164,#3165,#3166));
#884=EDGE_LOOP('',(#3167,#3168,#3169,#3170));
#885=EDGE_LOOP('',(#3171,#3172,#3173,#3174,#3175,#3176));
#886=EDGE_LOOP('',(#3177,#3178,#3179,#3180));
#887=EDGE_LOOP('',(#3181,#3182,#3183,#3184,#3185,#3186));
#888=EDGE_LOOP('',(#3187,#3188,#3189,#3190));
#889=EDGE_LOOP('',(#3191,#3192,#3193,#3194));
#890=EDGE_LOOP('',(#3195,#3196,#3197,#3198));
#891=EDGE_LOOP('',(#3199,#3200,#3201,#3202));
#892=EDGE_LOOP('',(#3203,#3204,#3205,#3206));
#893=EDGE_LOOP('',(#3207,#3208,#3209,#3210,#3211));
#894=EDGE_LOOP('',(#3212,#3213,#3214,#3215));
#895=EDGE_LOOP('',(#3216,#3217,#3218,#3219));
#896=EDGE_LOOP('',(#3220,#3221,#3222,#3223));
#897=EDGE_LOOP('',(#3224,#3225,#3226,#3227));
#898=EDGE_LOOP('',(#3228,#3229,#3230,#3231));
#899=EDGE_LOOP('',(#3232,#3233,#3234,#3235));
#900=EDGE_LOOP('',(#3236,#3237,#3238,#3239,#3240,#3241,#3242,#3243));
#901=EDGE_LOOP('',(#3244));
#902=EDGE_LOOP('',(#3245));
#903=EDGE_LOOP('',(#3246));
#904=EDGE_LOOP('',(#3247,#3248,#3249,#3250,#3251,#3252));
#905=EDGE_LOOP('',(#3253,#3254,#3255,#3256,#3257,#3258,#3259,#3260));
#906=EDGE_LOOP('',(#3261,#3262,#3263,#3264,#3265));
#907=EDGE_LOOP('',(#3266,#3267,#3268,#3269,#3270,#3271,#3272,#3273,#3274,
#3275,#3276,#3277,#3278));
#908=EDGE_LOOP('',(#3279,#3280,#3281,#3282,#3283,#3284));
#909=EDGE_LOOP('',(#3285,#3286,#3287,#3288,#3289,#3290));
#910=EDGE_LOOP('',(#3291,#3292,#3293,#3294,#3295,#3296));
#911=EDGE_LOOP('',(#3297,#3298,#3299,#3300,#3301,#3302,#3303,#3304));
#912=EDGE_LOOP('',(#3305));
#913=EDGE_LOOP('',(#3306));
#914=EDGE_LOOP('',(#3307));
#915=EDGE_LOOP('',(#3308,#3309,#3310));
#916=EDGE_LOOP('',(#3311,#3312));
#917=EDGE_LOOP('',(#3313,#3314,#3315,#3316));
#918=EDGE_LOOP('',(#3317,#3318,#3319,#3320));
#919=EDGE_LOOP('',(#3321,#3322,#3323,#3324,#3325,#3326,#3327,#3328,#3329,
#3330));
#920=EDGE_LOOP('',(#3331,#3332,#3333,#3334));
#921=EDGE_LOOP('',(#3335,#3336,#3337,#3338));
#922=EDGE_LOOP('',(#3339,#3340,#3341,#3342));
#923=EDGE_LOOP('',(#3343,#3344,#3345,#3346));
#924=EDGE_LOOP('',(#3347,#3348,#3349,#3350));
#925=EDGE_LOOP('',(#3351,#3352,#3353,#3354));
#926=EDGE_LOOP('',(#3355,#3356,#3357,#3358));
#927=EDGE_LOOP('',(#3359,#3360,#3361,#3362));
#928=EDGE_LOOP('',(#3363,#3364,#3365,#3366));
#929=EDGE_LOOP('',(#3367,#3368,#3369,#3370));
#930=EDGE_LOOP('',(#3371,#3372,#3373,#3374));
#931=EDGE_LOOP('',(#3375,#3376,#3377,#3378,#3379));
#932=EDGE_LOOP('',(#3380,#3381,#3382,#3383,#3384,#3385,#3386,#3387,#3388,
#3389,#3390,#3391,#3392,#3393,#3394));
#933=EDGE_LOOP('',(#3395,#3396,#3397,#3398,#3399));
#934=EDGE_LOOP('',(#3400,#3401,#3402,#3403));
#935=EDGE_LOOP('',(#3404,#3405,#3406,#3407,#3408,#3409,#3410,#3411,#3412,
#3413,#3414,#3415,#3416,#3417,#3418));
#936=EDGE_LOOP('',(#3419,#3420,#3421,#3422));
#937=EDGE_LOOP('',(#3423,#3424,#3425,#3426));
#938=EDGE_LOOP('',(#3427,#3428,#3429,#3430));
#939=EDGE_LOOP('',(#3431,#3432,#3433,#3434));
#940=EDGE_LOOP('',(#3435,#3436,#3437,#3438));
#941=EDGE_LOOP('',(#3439,#3440,#3441,#3442));
#942=EDGE_LOOP('',(#3443,#3444,#3445,#3446,#3447,#3448));
#943=EDGE_LOOP('',(#3449));
#944=EDGE_LOOP('',(#3450,#3451,#3452,#3453,#3454,#3455));
#945=EDGE_LOOP('',(#3456,#3457,#3458,#3459,#3460,#3461));
#946=EDGE_LOOP('',(#3462,#3463,#3464,#3465));
#947=EDGE_LOOP('',(#3466,#3467,#3468,#3469,#3470,#3471));
#948=EDGE_LOOP('',(#3472));
#949=EDGE_LOOP('',(#3473,#3474,#3475,#3476));
#950=EDGE_LOOP('',(#3477,#3478,#3479,#3480));
#951=EDGE_LOOP('',(#3481,#3482,#3483,#3484));
#952=EDGE_LOOP('',(#3485,#3486,#3487,#3488));
#953=EDGE_LOOP('',(#3489,#3490,#3491,#3492));
#954=EDGE_LOOP('',(#3493,#3494,#3495,#3496));
#955=EDGE_LOOP('',(#3497,#3498,#3499,#3500));
#956=EDGE_LOOP('',(#3501,#3502,#3503,#3504));
#957=EDGE_LOOP('',(#3505,#3506,#3507,#3508));
#958=EDGE_LOOP('',(#3509,#3510,#3511,#3512));
#959=EDGE_LOOP('',(#3513,#3514,#3515,#3516,#3517,#3518,#3519,#3520,#3521,
#3522,#3523,#3524,#3525,#3526));
#960=EDGE_LOOP('',(#3527,#3528,#3529,#3530,#3531));
#961=EDGE_LOOP('',(#3532,#3533,#3534,#3535));
#962=EDGE_LOOP('',(#3536,#3537,#3538,#3539,#3540,#3541,#3542,#3543,#3544,
#3545,#3546,#3547,#3548,#3549));
#963=EDGE_LOOP('',(#3550,#3551,#3552,#3553));
#964=EDGE_LOOP('',(#3554,#3555,#3556,#3557));
#965=EDGE_LOOP('',(#3558,#3559,#3560,#3561));
#966=EDGE_LOOP('',(#3562));
#967=EDGE_LOOP('',(#3563,#3564,#3565,#3566));
#968=EDGE_LOOP('',(#3567,#3568,#3569,#3570));
#969=EDGE_LOOP('',(#3571,#3572,#3573,#3574));
#970=EDGE_LOOP('',(#3575,#3576,#3577,#3578));
#971=EDGE_LOOP('',(#3579,#3580,#3581,#3582));
#972=EDGE_LOOP('',(#3583,#3584,#3585,#3586));
#973=EDGE_LOOP('',(#3587,#3588,#3589,#3590));
#974=EDGE_LOOP('',(#3591,#3592,#3593,#3594,#3595,#3596));
#975=EDGE_LOOP('',(#3597,#3598,#3599,#3600,#3601,#3602,#3603));
#976=EDGE_LOOP('',(#3604,#3605,#3606,#3607,#3608,#3609));
#977=EDGE_LOOP('',(#3610));
#978=EDGE_LOOP('',(#3611,#3612,#3613,#3614,#3615,#3616));
#979=EDGE_LOOP('',(#3617,#3618,#3619,#3620));
#980=EDGE_LOOP('',(#3621,#3622,#3623,#3624));
#981=EDGE_LOOP('',(#3625,#3626,#3627,#3628));
#982=EDGE_LOOP('',(#3629,#3630,#3631,#3632));
#983=EDGE_LOOP('',(#3633,#3634,#3635,#3636,#3637,#3638));
#984=EDGE_LOOP('',(#3639,#3640,#3641,#3642,#3643));
#985=EDGE_LOOP('',(#3644,#3645,#3646,#3647,#3648));
#986=EDGE_LOOP('',(#3649));
#987=EDGE_LOOP('',(#3650,#3651,#3652,#3653,#3654));
#988=EDGE_LOOP('',(#3655));
#989=EDGE_LOOP('',(#3656,#3657,#3658,#3659,#3660));
#990=EDGE_LOOP('',(#3661,#3662,#3663,#3664,#3665,#3666));
#991=EDGE_LOOP('',(#3667,#3668,#3669,#3670));
#992=EDGE_LOOP('',(#3671,#3672));
#993=EDGE_LOOP('',(#3673,#3674));
#994=EDGE_LOOP('',(#3675,#3676,#3677,#3678));
#995=EDGE_LOOP('',(#3679,#3680,#3681,#3682));
#996=EDGE_LOOP('',(#3683,#3684,#3685,#3686));
#997=EDGE_LOOP('',(#3687,#3688,#3689,#3690));
#998=EDGE_LOOP('',(#3691,#3692,#3693,#3694));
#999=EDGE_LOOP('',(#3695,#3696,#3697,#3698));
#1000=EDGE_LOOP('',(#3699,#3700,#3701,#3702));
#1001=EDGE_LOOP('',(#3703,#3704,#3705,#3706));
#1002=EDGE_LOOP('',(#3707,#3708,#3709,#3710));
#1003=EDGE_LOOP('',(#3711,#3712,#3713,#3714));
#1004=EDGE_LOOP('',(#3715,#3716,#3717,#3718));
#1005=EDGE_LOOP('',(#3719,#3720,#3721,#3722));
#1006=EDGE_LOOP('',(#3723,#3724,#3725,#3726));
#1007=EDGE_LOOP('',(#3727,#3728,#3729,#3730));
#1008=EDGE_LOOP('',(#3731,#3732,#3733,#3734));
#1009=EDGE_LOOP('',(#3735,#3736,#3737,#3738));
#1010=EDGE_LOOP('',(#3739,#3740,#3741,#3742));
#1011=EDGE_LOOP('',(#3743,#3744,#3745,#3746));
#1012=EDGE_LOOP('',(#3747,#3748,#3749,#3750));
#1013=EDGE_LOOP('',(#3751,#3752,#3753,#3754));
#1014=EDGE_LOOP('',(#3755,#3756,#3757,#3758));
#1015=EDGE_LOOP('',(#3759));
#1016=EDGE_LOOP('',(#3760,#3761,#3762,#3763));
#1017=EDGE_LOOP('',(#3764,#3765,#3766,#3767));
#1018=EDGE_LOOP('',(#3768,#3769,#3770,#3771));
#1019=EDGE_LOOP('',(#3772,#3773,#3774,#3775));
#1020=EDGE_LOOP('',(#3776,#3777,#3778,#3779));
#1021=EDGE_LOOP('',(#3780,#3781,#3782,#3783,#3784,#3785,#3786,#3787,#3788,
#3789));
#1022=EDGE_LOOP('',(#3790));
#1023=EDGE_LOOP('',(#3791,#3792,#3793,#3794));
#1024=EDGE_LOOP('',(#3795,#3796,#3797,#3798));
#1025=EDGE_LOOP('',(#3799,#3800,#3801,#3802));
#1026=EDGE_LOOP('',(#3803,#3804,#3805,#3806));
#1027=EDGE_LOOP('',(#3807,#3808,#3809,#3810));
#1028=EDGE_LOOP('',(#3811,#3812,#3813,#3814,#3815,#3816,#3817,#3818,#3819,
#3820));
#1029=EDGE_LOOP('',(#3821));
#1030=EDGE_LOOP('',(#3822,#3823,#3824,#3825));
#1031=EDGE_LOOP('',(#3826));
#1032=EDGE_LOOP('',(#3827,#3828,#3829,#3830));
#1033=EDGE_LOOP('',(#3831));
#1034=EDGE_LOOP('',(#3832));
#1035=EDGE_LOOP('',(#3833,#3834,#3835,#3836));
#1036=EDGE_LOOP('',(#3837));
#1037=EDGE_LOOP('',(#3838));
#1038=EDGE_LOOP('',(#3839,#3840,#3841,#3842));
#1039=EDGE_LOOP('',(#3843));
#1040=EDGE_LOOP('',(#3844));
#1041=EDGE_LOOP('',(#3845,#3846,#3847,#3848));
#1042=EDGE_LOOP('',(#3849,#3850,#3851,#3852));
#1043=EDGE_LOOP('',(#3853,#3854,#3855,#3856));
#1044=EDGE_LOOP('',(#3857,#3858,#3859,#3860));
#1045=EDGE_LOOP('',(#3861,#3862,#3863,#3864));
#1046=EDGE_LOOP('',(#3865,#3866,#3867,#3868));
#1047=EDGE_LOOP('',(#3869,#3870,#3871,#3872));
#1048=EDGE_LOOP('',(#3873,#3874,#3875,#3876));
#1049=EDGE_LOOP('',(#3877,#3878,#3879,#3880));
#1050=EDGE_LOOP('',(#3881,#3882,#3883,#3884));
#1051=EDGE_LOOP('',(#3885,#3886,#3887,#3888));
#1052=EDGE_LOOP('',(#3889,#3890,#3891,#3892));
#1053=EDGE_LOOP('',(#3893,#3894,#3895,#3896));
#1054=EDGE_LOOP('',(#3897,#3898,#3899,#3900));
#1055=EDGE_LOOP('',(#3901,#3902,#3903,#3904));
#1056=EDGE_LOOP('',(#3905,#3906,#3907,#3908));
#1057=EDGE_LOOP('',(#3909,#3910,#3911,#3912));
#1058=EDGE_LOOP('',(#3913,#3914,#3915,#3916));
#1059=EDGE_LOOP('',(#3917,#3918,#3919,#3920));
#1060=EDGE_LOOP('',(#3921,#3922,#3923,#3924));
#1061=EDGE_LOOP('',(#3925,#3926,#3927,#3928));
#1062=EDGE_LOOP('',(#3929,#3930,#3931,#3932));
#1063=EDGE_LOOP('',(#3933,#3934,#3935,#3936));
#1064=EDGE_LOOP('',(#3937,#3938,#3939,#3940));
#1065=EDGE_LOOP('',(#3941,#3942,#3943,#3944,#3945,#3946,#3947,#3948,#3949,
#3950,#3951,#3952,#3953,#3954,#3955,#3956,#3957,#3958,#3959,#3960,#3961,
#3962,#3963,#3964,#3965,#3966,#3967,#3968));
#1066=EDGE_LOOP('',(#3969,#3970,#3971,#3972,#3973));
#1067=EDGE_LOOP('',(#3974,#3975,#3976,#3977));
#1068=EDGE_LOOP('',(#3978,#3979,#3980,#3981,#3982,#3983,#3984,#3985,#3986,
#3987,#3988,#3989,#3990,#3991,#3992,#3993,#3994,#3995,#3996,#3997,#3998,
#3999,#4000,#4001,#4002,#4003,#4004,#4005));
#1069=EDGE_LOOP('',(#4006,#4007,#4008,#4009));
#1070=EDGE_LOOP('',(#4010,#4011,#4012,#4013));
#1071=EDGE_LOOP('',(#4014,#4015,#4016,#4017));
#1072=EDGE_LOOP('',(#4018,#4019,#4020,#4021));
#1073=EDGE_LOOP('',(#4022,#4023,#4024,#4025));
#1074=EDGE_LOOP('',(#4026,#4027,#4028,#4029));
#1075=EDGE_LOOP('',(#4030,#4031,#4032,#4033));
#1076=EDGE_LOOP('',(#4034));
#1077=EDGE_LOOP('',(#4035,#4036,#4037,#4038,#4039,#4040,#4041,#4042,#4043,
#4044,#4045,#4046));
#1078=EDGE_LOOP('',(#4047,#4048,#4049,#4050));
#1079=EDGE_LOOP('',(#4051,#4052,#4053,#4054));
#1080=EDGE_LOOP('',(#4055,#4056,#4057,#4058));
#1081=EDGE_LOOP('',(#4059,#4060,#4061,#4062));
#1082=EDGE_LOOP('',(#4063,#4064,#4065,#4066));
#1083=EDGE_LOOP('',(#4067,#4068,#4069,#4070,#4071,#4072,#4073,#4074,#4075,
#4076,#4077,#4078));
#1084=EDGE_LOOP('',(#4079));
#1085=EDGE_LOOP('',(#4080,#4081,#4082,#4083,#4084,#4085));
#1086=EDGE_LOOP('',(#4086,#4087,#4088,#4089));
#1087=EDGE_LOOP('',(#4090));
#1088=EDGE_LOOP('',(#4091,#4092,#4093,#4094));
#1089=EDGE_LOOP('',(#4095,#4096,#4097,#4098));
#1090=EDGE_LOOP('',(#4099,#4100,#4101,#4102));
#1091=EDGE_LOOP('',(#4103,#4104,#4105,#4106,#4107));
#1092=EDGE_LOOP('',(#4108,#4109,#4110,#4111,#4112,#4113));
#1093=EDGE_LOOP('',(#4114));
#1094=EDGE_LOOP('',(#4115));
#1095=EDGE_LOOP('',(#4116,#4117,#4118,#4119,#4120));
#1096=EDGE_LOOP('',(#4121));
#1097=EDGE_LOOP('',(#4122));
#1098=EDGE_LOOP('',(#4123,#4124,#4125,#4126));
#1099=EDGE_LOOP('',(#4127,#4128,#4129,#4130));
#1100=EDGE_LOOP('',(#4131,#4132,#4133,#4134));
#1101=LINE('',#6333,#1391);
#1102=LINE('',#6337,#1392);
#1103=LINE('',#6348,#1393);
#1104=LINE('',#6353,#1394);
#1105=LINE('',#6357,#1395);
#1106=LINE('',#6361,#1396);
#1107=LINE('',#6365,#1397);
#1108=LINE('',#6370,#1398);
#1109=LINE('',#6375,#1399);
#1110=LINE('',#6380,#1400);
#1111=LINE('',#6384,#1401);
#1112=LINE('',#6388,#1402);
#1113=LINE('',#6392,#1403);
#1114=LINE('',#6396,#1404);
#1115=LINE('',#6400,#1405);
#1116=LINE('',#6402,#1406);
#1117=LINE('',#6403,#1407);
#1118=LINE('',#6406,#1408);
#1119=LINE('',#6410,#1409);
#1120=LINE('',#6411,#1410);
#1121=LINE('',#6414,#1411);
#1122=LINE('',#6418,#1412);
#1123=LINE('',#6419,#1413);
#1124=LINE('',#6422,#1414);
#1125=LINE('',#6426,#1415);
#1126=LINE('',#6427,#1416);
#1127=LINE('',#6432,#1417);
#1128=LINE('',#6435,#1418);
#1129=LINE('',#6438,#1419);
#1130=LINE('',#6439,#1420);
#1131=LINE('',#6441,#1421);
#1132=LINE('',#6443,#1422);
#1133=LINE('',#6446,#1423);
#1134=LINE('',#6449,#1424);
#1135=LINE('',#6450,#1425);
#1136=LINE('',#6451,#1426);
#1137=LINE('',#6454,#1427);
#1138=LINE('',#6458,#1428);
#1139=LINE('',#6459,#1429);
#1140=LINE('',#6462,#1430);
#1141=LINE('',#6465,#1431);
#1142=LINE('',#6466,#1432);
#1143=LINE('',#6468,#1433);
#1144=LINE('',#6470,#1434);
#1145=LINE('',#6473,#1435);
#1146=LINE('',#6474,#1436);
#1147=LINE('',#6476,#1437);
#1148=LINE('',#6478,#1438);
#1149=LINE('',#6482,#1439);
#1150=LINE('',#6490,#1440);
#1151=LINE('',#6499,#1441);
#1152=LINE('',#6505,#1442);
#1153=LINE('',#6508,#1443);
#1154=LINE('',#6515,#1444);
#1155=LINE('',#6519,#1445);
#1156=LINE('',#6523,#1446);
#1157=LINE('',#6530,#1447);
#1158=LINE('',#6534,#1448);
#1159=LINE('',#6541,#1449);
#1160=LINE('',#6548,#1450);
#1161=LINE('',#6556,#1451);
#1162=LINE('',#6560,#1452);
#1163=LINE('',#6564,#1453);
#1164=LINE('',#6570,#1454);
#1165=LINE('',#6578,#1455);
#1166=LINE('',#6584,#1456);
#1167=LINE('',#6588,#1457);
#1168=LINE('',#6592,#1458);
#1169=LINE('',#6600,#1459);
#1170=LINE('',#6608,#1460);
#1171=LINE('',#6618,#1461);
#1172=LINE('',#6623,#1462);
#1173=LINE('',#6630,#1463);
#1174=LINE('',#6632,#1464);
#1175=LINE('',#6634,#1465);
#1176=LINE('',#6645,#1466);
#1177=LINE('',#6650,#1467);
#1178=LINE('',#6657,#1468);
#1179=LINE('',#6659,#1469);
#1180=LINE('',#6661,#1470);
#1181=LINE('',#6672,#1471);
#1182=LINE('',#6677,#1472);
#1183=LINE('',#6684,#1473);
#1184=LINE('',#6686,#1474);
#1185=LINE('',#6688,#1475);
#1186=LINE('',#6699,#1476);
#1187=LINE('',#6704,#1477);
#1188=LINE('',#6711,#1478);
#1189=LINE('',#6713,#1479);
#1190=LINE('',#6715,#1480);
#1191=LINE('',#6722,#1481);
#1192=LINE('',#6753,#1482);
#1193=LINE('',#6756,#1483);
#1194=LINE('',#6773,#1484);
#1195=LINE('',#6852,#1485);
#1196=LINE('',#6906,#1486);
#1197=LINE('',#6915,#1487);
#1198=LINE('',#6917,#1488);
#1199=LINE('',#6919,#1489);
#1200=LINE('',#6921,#1490);
#1201=LINE('',#6923,#1491);
#1202=LINE('',#6928,#1492);
#1203=LINE('',#6952,#1493);
#1204=LINE('',#7000,#1494);
#1205=LINE('',#7048,#1495);
#1206=LINE('',#7096,#1496);
#1207=LINE('',#7150,#1497);
#1208=LINE('',#7198,#1498);
#1209=LINE('',#7220,#1499);
#1210=LINE('',#7245,#1500);
#1211=LINE('',#7270,#1501);
#1212=LINE('',#7294,#1502);
#1213=LINE('',#7970,#1503);
#1214=LINE('',#7972,#1504);
#1215=LINE('',#7974,#1505);
#1216=LINE('',#7975,#1506);
#1217=LINE('',#7978,#1507);
#1218=LINE('',#7980,#1508);
#1219=LINE('',#7981,#1509);
#1220=LINE('',#7984,#1510);
#1221=LINE('',#7986,#1511);
#1222=LINE('',#7987,#1512);
#1223=LINE('',#7990,#1513);
#1224=LINE('',#7992,#1514);
#1225=LINE('',#7993,#1515);
#1226=LINE('',#7996,#1516);
#1227=LINE('',#7998,#1517);
#1228=LINE('',#7999,#1518);
#1229=LINE('',#8001,#1519);
#1230=LINE('',#8002,#1520);
#1231=LINE('',#8008,#1521);
#1232=LINE('',#8014,#1522);
#1233=LINE('',#8020,#1523);
#1234=LINE('',#8044,#1524);
#1235=LINE('',#8092,#1525);
#1236=LINE('',#8143,#1526);
#1237=LINE('',#8194,#1527);
#1238=LINE('',#8242,#1528);
#1239=LINE('',#8259,#1529);
#1240=LINE('',#8284,#1530);
#1241=LINE('',#8308,#1531);
#1242=LINE('',#8334,#1532);
#1243=LINE('',#9026,#1533);
#1244=LINE('',#9028,#1534);
#1245=LINE('',#9030,#1535);
#1246=LINE('',#9031,#1536);
#1247=LINE('',#9035,#1537);
#1248=LINE('',#9037,#1538);
#1249=LINE('',#9039,#1539);
#1250=LINE('',#9040,#1540);
#1251=LINE('',#9053,#1541);
#1252=LINE('',#9055,#1542);
#1253=LINE('',#9056,#1543);
#1254=LINE('',#9061,#1544);
#1255=LINE('',#9062,#1545);
#1256=LINE('',#9067,#1546);
#1257=LINE('',#9068,#1547);
#1258=LINE('',#9073,#1548);
#1259=LINE('',#9074,#1549);
#1260=LINE('',#9079,#1550);
#1261=LINE('',#9080,#1551);
#1262=LINE('',#9083,#1552);
#1263=LINE('',#9100,#1553);
#1264=LINE('',#9107,#1554);
#1265=LINE('',#9113,#1555);
#1266=LINE('',#9119,#1556);
#1267=LINE('',#9128,#1557);
#1268=LINE('',#9134,#1558);
#1269=LINE('',#9175,#1559);
#1270=LINE('',#9214,#1560);
#1271=LINE('',#9219,#1561);
#1272=LINE('',#9221,#1562);
#1273=LINE('',#9223,#1563);
#1274=LINE('',#9224,#1564);
#1275=LINE('',#9229,#1565);
#1276=LINE('',#9233,#1566);
#1277=LINE('',#9235,#1567);
#1278=LINE('',#9236,#1568);
#1279=LINE('',#9241,#1569);
#1280=LINE('',#9245,#1570);
#1281=LINE('',#9247,#1571);
#1282=LINE('',#9248,#1572);
#1283=LINE('',#9253,#1573);
#1284=LINE('',#9258,#1574);
#1285=LINE('',#9259,#1575);
#1286=LINE('',#9260,#1576);
#1287=LINE('',#9265,#1577);
#1288=LINE('',#9270,#1578);
#1289=LINE('',#9277,#1579);
#1290=LINE('',#9282,#1580);
#1291=LINE('',#9283,#1581);
#1292=LINE('',#9284,#1582);
#1293=LINE('',#9289,#1583);
#1294=LINE('',#9294,#1584);
#1295=LINE('',#9295,#1585);
#1296=LINE('',#9296,#1586);
#1297=LINE('',#9300,#1587);
#1298=LINE('',#9306,#1588);
#1299=LINE('',#9307,#1589);
#1300=LINE('',#9308,#1590);
#1301=LINE('',#9313,#1591);
#1302=LINE('',#9317,#1592);
#1303=LINE('',#9319,#1593);
#1304=LINE('',#9320,#1594);
#1305=LINE('',#9325,#1595);
#1306=LINE('',#9331,#1596);
#1307=LINE('',#9337,#1597);
#1308=LINE('',#9341,#1598);
#1309=LINE('',#9342,#1599);
#1310=LINE('',#9344,#1600);
#1311=LINE('',#9346,#1601);
#1312=LINE('',#9348,#1602);
#1313=LINE('',#9351,#1603);
#1314=LINE('',#9355,#1604);
#1315=LINE('',#9357,#1605);
#1316=LINE('',#9359,#1606);
#1317=LINE('',#9362,#1607);
#1318=LINE('',#9366,#1608);
#1319=LINE('',#9375,#1609);
#1320=LINE('',#9383,#1610);
#1321=LINE('',#9390,#1611);
#1322=LINE('',#9396,#1612);
#1323=LINE('',#9420,#1613);
#1324=LINE('',#9468,#1614);
#1325=LINE('',#9516,#1615);
#1326=LINE('',#9564,#1616);
#1327=LINE('',#9618,#1617);
#1328=LINE('',#9666,#1618);
#1329=LINE('',#9714,#1619);
#1330=LINE('',#9768,#1620);
#1331=LINE('',#9816,#1621);
#1332=LINE('',#9864,#1622);
#1333=LINE('',#9912,#1623);
#1334=LINE('',#9966,#1624);
#1335=LINE('',#9984,#1625);
#1336=LINE('',#10009,#1626);
#1337=LINE('',#10034,#1627);
#1338=LINE('',#10058,#1628);
#1339=LINE('',#10082,#1629);
#1340=LINE('',#10107,#1630);
#1341=LINE('',#10132,#1631);
#1342=LINE('',#10156,#1632);
#1343=LINE('',#10181,#1633);
#1344=LINE('',#10206,#1634);
#1345=LINE('',#10230,#1635);
#1346=LINE('',#11262,#1636);
#1347=LINE('',#11264,#1637);
#1348=LINE('',#11266,#1638);
#1349=LINE('',#11267,#1639);
#1350=LINE('',#11271,#1640);
#1351=LINE('',#11273,#1641);
#1352=LINE('',#11275,#1642);
#1353=LINE('',#11276,#1643);
#1354=LINE('',#11280,#1644);
#1355=LINE('',#11282,#1645);
#1356=LINE('',#11284,#1646);
#1357=LINE('',#11285,#1647);
#1358=LINE('',#11288,#1648);
#1359=LINE('',#11290,#1649);
#1360=LINE('',#11291,#1650);
#1361=LINE('',#11295,#1651);
#1362=LINE('',#11296,#1652);
#1363=LINE('',#11297,#1653);
#1364=LINE('',#11299,#1654);
#1365=LINE('',#11300,#1655);
#1366=LINE('',#11303,#1656);
#1367=LINE('',#11305,#1657);
#1368=LINE('',#11306,#1658);
#1369=LINE('',#11311,#1659);
#1370=LINE('',#11312,#1660);
#1371=LINE('',#11314,#1661);
#1372=LINE('',#11316,#1662);
#1373=LINE('',#11317,#1663);
#1374=LINE('',#11320,#1664);
#1375=LINE('',#11321,#1665);
#1376=LINE('',#11323,#1666);
#1377=LINE('',#11326,#1667);
#1378=LINE('',#11327,#1668);
#1379=LINE('',#11330,#1669);
#1380=LINE('',#11331,#1670);
#1381=LINE('',#11333,#1671);
#1382=LINE('',#11339,#1672);
#1383=LINE('',#11348,#1673);
#1384=LINE('',#11350,#1674);
#1385=LINE('',#11356,#1675);
#1386=LINE('',#11365,#1676);
#1387=LINE('',#11371,#1677);
#1388=LINE('',#11379,#1678);
#1389=LINE('',#11383,#1679);
#1390=LINE('',#11385,#1680);
#1391=VECTOR('',#5091,2.82);
#1392=VECTOR('',#5096,3.);
#1393=VECTOR('',#5109,5.105);
#1394=VECTOR('',#5114,10.);
#1395=VECTOR('',#5117,10.);
#1396=VECTOR('',#5120,10.);
#1397=VECTOR('',#5123,10.);
#1398=VECTOR('',#5130,5.005);
#1399=VECTOR('',#5135,5.105);
#1400=VECTOR('',#5140,10.);
#1401=VECTOR('',#5143,10.);
#1402=VECTOR('',#5146,10.);
#1403=VECTOR('',#5149,10.);
#1404=VECTOR('',#5154,5.005);
#1405=VECTOR('',#5159,10.);
#1406=VECTOR('',#5160,10.);
#1407=VECTOR('',#5161,10.);
#1408=VECTOR('',#5164,10.);
#1409=VECTOR('',#5169,10.);
#1410=VECTOR('',#5170,10.);
#1411=VECTOR('',#5173,10.);
#1412=VECTOR('',#5178,10.);
#1413=VECTOR('',#5179,10.);
#1414=VECTOR('',#5182,10.);
#1415=VECTOR('',#5187,10.);
#1416=VECTOR('',#5188,10.);
#1417=VECTOR('',#5195,10.);
#1418=VECTOR('',#5198,10.);
#1419=VECTOR('',#5201,10.);
#1420=VECTOR('',#5202,10.);
#1421=VECTOR('',#5205,10.);
#1422=VECTOR('',#5206,10.);
#1423=VECTOR('',#5211,10.);
#1424=VECTOR('',#5214,10.);
#1425=VECTOR('',#5215,10.);
#1426=VECTOR('',#5216,10.);
#1427=VECTOR('',#5219,10.);
#1428=VECTOR('',#5224,10.);
#1429=VECTOR('',#5225,10.);
#1430=VECTOR('',#5228,10.);
#1431=VECTOR('',#5233,10.);
#1432=VECTOR('',#5234,10.);
#1433=VECTOR('',#5237,10.);
#1434=VECTOR('',#5240,10.);
#1435=VECTOR('',#5245,10.);
#1436=VECTOR('',#5246,10.);
#1437=VECTOR('',#5249,10.);
#1438=VECTOR('',#5252,10.);
#1439=VECTOR('',#5257,1.3);
#1440=VECTOR('',#5268,4.25);
#1441=VECTOR('',#5281,2.6575);
#1442=VECTOR('',#5288,2.6575);
#1443=VECTOR('',#5293,2.515);
#1444=VECTOR('',#5302,3.85);
#1445=VECTOR('',#5307,4.);
#1446=VECTOR('',#5312,3.9);
#1447=VECTOR('',#5321,3.);
#1448=VECTOR('',#5326,2.9);
#1449=VECTOR('',#5335,3.825);
#1450=VECTOR('',#5344,4.275);
#1451=VECTOR('',#5355,4.925);
#1452=VECTOR('',#5360,5.);
#1453=VECTOR('',#5365,4.925);
#1454=VECTOR('',#5372,4.275);
#1455=VECTOR('',#5383,3.825);
#1456=VECTOR('',#5390,3.075);
#1457=VECTOR('',#5395,3.);
#1458=VECTOR('',#5400,3.075);
#1459=VECTOR('',#5411,3.05);
#1460=VECTOR('',#5422,4.);
#1461=VECTOR('',#5429,10.);
#1462=VECTOR('',#5430,10.);
#1463=VECTOR('',#5433,10.);
#1464=VECTOR('',#5434,10.);
#1465=VECTOR('',#5435,10.);
#1466=VECTOR('',#5438,10.);
#1467=VECTOR('',#5439,10.);
#1468=VECTOR('',#5442,10.);
#1469=VECTOR('',#5443,10.);
#1470=VECTOR('',#5444,10.);
#1471=VECTOR('',#5447,10.);
#1472=VECTOR('',#5448,10.);
#1473=VECTOR('',#5451,10.);
#1474=VECTOR('',#5452,10.);
#1475=VECTOR('',#5453,10.);
#1476=VECTOR('',#5456,10.);
#1477=VECTOR('',#5457,10.);
#1478=VECTOR('',#5460,10.);
#1479=VECTOR('',#5461,10.);
#1480=VECTOR('',#5462,10.);
#1481=VECTOR('',#5465,10.);
#1482=VECTOR('',#5480,10.);
#1483=VECTOR('',#5483,10.);
#1484=VECTOR('',#5494,10.);
#1485=VECTOR('',#5539,1.05);
#1486=VECTOR('',#5558,3.16);
#1487=VECTOR('',#5571,10.);
#1488=VECTOR('',#5574,10.);
#1489=VECTOR('',#5577,1.52);
#1490=VECTOR('',#5580,1.52);
#1491=VECTOR('',#5583,3.01);
#1492=VECTOR('',#5588,1.);
#1493=VECTOR('',#5593,1.);
#1494=VECTOR('',#5596,1.);
#1495=VECTOR('',#5599,1.);
#1496=VECTOR('',#5602,1.);
#1497=VECTOR('',#5605,1.);
#1498=VECTOR('',#5608,0.739);
#1499=VECTOR('',#5613,0.739);
#1500=VECTOR('',#5616,0.739);
#1501=VECTOR('',#5619,0.739);
#1502=VECTOR('',#5622,0.739);
#1503=VECTOR('',#5641,10.);
#1504=VECTOR('',#5642,10.);
#1505=VECTOR('',#5643,10.);
#1506=VECTOR('',#5644,10.);
#1507=VECTOR('',#5647,10.);
#1508=VECTOR('',#5648,10.);
#1509=VECTOR('',#5649,10.);
#1510=VECTOR('',#5652,10.);
#1511=VECTOR('',#5653,10.);
#1512=VECTOR('',#5654,10.);
#1513=VECTOR('',#5657,10.);
#1514=VECTOR('',#5658,10.);
#1515=VECTOR('',#5659,10.);
#1516=VECTOR('',#5662,10.);
#1517=VECTOR('',#5663,10.);
#1518=VECTOR('',#5664,10.);
#1519=VECTOR('',#5667,10.);
#1520=VECTOR('',#5668,10.);
#1521=VECTOR('',#5677,0.9);
#1522=VECTOR('',#5686,0.875);
#1523=VECTOR('',#5693,1.25);
#1524=VECTOR('',#5698,1.25);
#1525=VECTOR('',#5701,1.25);
#1526=VECTOR('',#5704,1.25);
#1527=VECTOR('',#5707,1.25);
#1528=VECTOR('',#5710,0.95825);
#1529=VECTOR('',#5715,0.95825);
#1530=VECTOR('',#5718,0.95825);
#1531=VECTOR('',#5721,0.95825);
#1532=VECTOR('',#5724,0.95825);
#1533=VECTOR('',#5737,10.);
#1534=VECTOR('',#5738,10.);
#1535=VECTOR('',#5739,10.);
#1536=VECTOR('',#5740,10.);
#1537=VECTOR('',#5743,10.);
#1538=VECTOR('',#5744,10.);
#1539=VECTOR('',#5745,10.);
#1540=VECTOR('',#5746,10.);
#1541=VECTOR('',#5763,10.);
#1542=VECTOR('',#5764,10.);
#1543=VECTOR('',#5765,10.);
#1544=VECTOR('',#5770,10.);
#1545=VECTOR('',#5771,10.);
#1546=VECTOR('',#5776,10.);
#1547=VECTOR('',#5777,10.);
#1548=VECTOR('',#5782,10.);
#1549=VECTOR('',#5783,10.);
#1550=VECTOR('',#5788,10.);
#1551=VECTOR('',#5789,10.);
#1552=VECTOR('',#5794,10.);
#1553=VECTOR('',#5815,1.15);
#1554=VECTOR('',#5828,1.5);
#1555=VECTOR('',#5835,2.07071067811866);
#1556=VECTOR('',#5842,2.3);
#1557=VECTOR('',#5853,2.07071067811866);
#1558=VECTOR('',#5862,2.3);
#1559=VECTOR('',#5865,0.800000000000001);
#1560=VECTOR('',#5868,2.5);
#1561=VECTOR('',#5873,10.);
#1562=VECTOR('',#5874,10.);
#1563=VECTOR('',#5875,10.);
#1564=VECTOR('',#5876,10.);
#1565=VECTOR('',#5881,10.);
#1566=VECTOR('',#5886,10.);
#1567=VECTOR('',#5887,10.);
#1568=VECTOR('',#5888,10.);
#1569=VECTOR('',#5893,10.);
#1570=VECTOR('',#5898,10.);
#1571=VECTOR('',#5899,10.);
#1572=VECTOR('',#5900,10.);
#1573=VECTOR('',#5905,10.);
#1574=VECTOR('',#5910,10.);
#1575=VECTOR('',#5911,10.);
#1576=VECTOR('',#5912,10.);
#1577=VECTOR('',#5917,10.);
#1578=VECTOR('',#5922,10.);
#1579=VECTOR('',#5931,10.);
#1580=VECTOR('',#5936,10.);
#1581=VECTOR('',#5937,10.);
#1582=VECTOR('',#5938,10.);
#1583=VECTOR('',#5943,10.);
#1584=VECTOR('',#5948,10.);
#1585=VECTOR('',#5949,10.);
#1586=VECTOR('',#5950,10.);
#1587=VECTOR('',#5953,10.);
#1588=VECTOR('',#5960,10.);
#1589=VECTOR('',#5961,10.);
#1590=VECTOR('',#5962,10.);
#1591=VECTOR('',#5967,10.);
#1592=VECTOR('',#5972,10.);
#1593=VECTOR('',#5973,10.);
#1594=VECTOR('',#5974,10.);
#1595=VECTOR('',#5979,10.);
#1596=VECTOR('',#5986,10.);
#1597=VECTOR('',#5997,10.);
#1598=VECTOR('',#6002,10.);
#1599=VECTOR('',#6003,10.);
#1600=VECTOR('',#6006,10.);
#1601=VECTOR('',#6009,10.);
#1602=VECTOR('',#6012,10.);
#1603=VECTOR('',#6017,10.);
#1604=VECTOR('',#6022,10.);
#1605=VECTOR('',#6025,10.);
#1606=VECTOR('',#6028,10.);
#1607=VECTOR('',#6031,2.01);
#1608=VECTOR('',#6036,1.05);
#1609=VECTOR('',#6049,1.05);
#1610=VECTOR('',#6060,1.5);
#1611=VECTOR('',#6069,2.25);
#1612=VECTOR('',#6076,1.);
#1613=VECTOR('',#6081,1.);
#1614=VECTOR('',#6084,1.);
#1615=VECTOR('',#6087,1.);
#1616=VECTOR('',#6090,1.);
#1617=VECTOR('',#6093,1.);
#1618=VECTOR('',#6096,1.);
#1619=VECTOR('',#6099,1.);
#1620=VECTOR('',#6102,1.);
#1621=VECTOR('',#6105,1.);
#1622=VECTOR('',#6108,1.);
#1623=VECTOR('',#6111,1.);
#1624=VECTOR('',#6114,0.739);
#1625=VECTOR('',#6119,0.739);
#1626=VECTOR('',#6122,0.739);
#1627=VECTOR('',#6125,0.739);
#1628=VECTOR('',#6128,0.739);
#1629=VECTOR('',#6131,0.739);
#1630=VECTOR('',#6134,0.739);
#1631=VECTOR('',#6137,0.739);
#1632=VECTOR('',#6140,0.739);
#1633=VECTOR('',#6143,0.739);
#1634=VECTOR('',#6146,0.739);
#1635=VECTOR('',#6149,0.739);
#1636=VECTOR('',#6162,10.);
#1637=VECTOR('',#6163,10.);
#1638=VECTOR('',#6164,10.);
#1639=VECTOR('',#6165,10.);
#1640=VECTOR('',#6168,10.);
#1641=VECTOR('',#6169,10.);
#1642=VECTOR('',#6170,10.);
#1643=VECTOR('',#6171,10.);
#1644=VECTOR('',#6174,10.);
#1645=VECTOR('',#6175,10.);
#1646=VECTOR('',#6176,10.);
#1647=VECTOR('',#6177,10.);
#1648=VECTOR('',#6180,10.);
#1649=VECTOR('',#6181,10.);
#1650=VECTOR('',#6182,10.);
#1651=VECTOR('',#6185,10.);
#1652=VECTOR('',#6186,10.);
#1653=VECTOR('',#6187,10.);
#1654=VECTOR('',#6190,10.);
#1655=VECTOR('',#6191,10.);
#1656=VECTOR('',#6194,10.);
#1657=VECTOR('',#6195,10.);
#1658=VECTOR('',#6196,10.);
#1659=VECTOR('',#6201,10.);
#1660=VECTOR('',#6202,10.);
#1661=VECTOR('',#6203,10.);
#1662=VECTOR('',#6204,10.);
#1663=VECTOR('',#6205,10.);
#1664=VECTOR('',#6208,10.);
#1665=VECTOR('',#6209,10.);
#1666=VECTOR('',#6212,10.);
#1667=VECTOR('',#6215,10.);
#1668=VECTOR('',#6216,10.);
#1669=VECTOR('',#6219,10.);
#1670=VECTOR('',#6220,10.);
#1671=VECTOR('',#6223,10.);
#1672=VECTOR('',#6232,0.9);
#1673=VECTOR('',#6245,2.);
#1674=VECTOR('',#6248,1.8);
#1675=VECTOR('',#6255,1.35);
#1676=VECTOR('',#6266,1.25);
#1677=VECTOR('',#6273,1.35);
#1678=VECTOR('',#6284,1.9);
#1679=VECTOR('',#6289,2.);
#1680=VECTOR('',#6292,1.9);
#1681=CIRCLE('',#4609,2.64);
#1682=CIRCLE('',#4610,3.);
#1683=CIRCLE('',#4612,3.);
#1684=CIRCLE('',#4613,3.);
#1685=CIRCLE('',#4615,1.3);
#1686=CIRCLE('',#4617,5.205);
#1687=CIRCLE('',#4618,5.005);
#1688=CIRCLE('',#4620,3.6);
#1689=CIRCLE('',#4621,3.6);
#1690=CIRCLE('',#4622,3.6);
#1691=CIRCLE('',#4623,3.6);
#1692=CIRCLE('',#4625,5.005);
#1693=CIRCLE('',#4627,5.205);
#1694=CIRCLE('',#4628,5.005);
#1695=CIRCLE('',#4630,3.6);
#1696=CIRCLE('',#4631,3.6);
#1697=CIRCLE('',#4632,3.6);
#1698=CIRCLE('',#4633,3.6);
#1699=CIRCLE('',#4635,5.005);
#1700=CIRCLE('',#4638,4.);
#1701=CIRCLE('',#4641,4.);
#1702=CIRCLE('',#4644,4.);
#1703=CIRCLE('',#4647,4.);
#1704=CIRCLE('',#4649,4.);
#1705=CIRCLE('',#4652,4.);
#1706=CIRCLE('',#4656,4.);
#1707=CIRCLE('',#4659,4.);
#1708=CIRCLE('',#4669,1.3);
#1709=CIRCLE('',#4672,4.25);
#1710=CIRCLE('',#4674,4.25);
#1711=CIRCLE('',#4679,2.515);
#1712=CIRCLE('',#4680,2.71857142857143);
#1713=CIRCLE('',#4682,2.71857142857143);
#1714=CIRCLE('',#4683,2.515);
#1715=CIRCLE('',#4686,3.7);
#1716=CIRCLE('',#4688,4.);
#1717=CIRCLE('',#4690,4.);
#1718=CIRCLE('',#4692,3.8);
#1719=CIRCLE('',#4694,3.);
#1720=CIRCLE('',#4696,3.);
#1721=CIRCLE('',#4698,2.8);
#1722=CIRCLE('',#4702,3.85);
#1723=CIRCLE('',#4703,3.8);
#1724=CIRCLE('',#4705,4.25);
#1725=CIRCLE('',#4707,4.3);
#1726=CIRCLE('',#4709,4.85);
#1727=CIRCLE('',#4711,5.);
#1728=CIRCLE('',#4713,5.);
#1729=CIRCLE('',#4715,4.85);
#1730=CIRCLE('',#4717,4.3);
#1731=CIRCLE('',#4719,4.25);
#1732=CIRCLE('',#4721,3.85);
#1733=CIRCLE('',#4723,3.8);
#1734=CIRCLE('',#4725,3.15);
#1735=CIRCLE('',#4727,3.);
#1736=CIRCLE('',#4729,3.);
#1737=CIRCLE('',#4731,3.15);
#1738=CIRCLE('',#4735,3.05);
#1739=CIRCLE('',#4736,3.05);
#1740=CIRCLE('',#4738,4.);
#1741=CIRCLE('',#4740,4.);
#1742=CIRCLE('',#4753,5.3);
#1743=CIRCLE('',#4754,5.5);
#1744=CIRCLE('',#4756,3.);
#1745=CIRCLE('',#4757,2.8);
#1746=CIRCLE('',#4761,5.5);
#1747=CIRCLE('',#4762,5.5);
#1748=CIRCLE('',#4763,5.3);
#1749=CIRCLE('',#4766,3.);
#1750=CIRCLE('',#4767,2.8);
#1751=CIRCLE('',#4769,3.);
#1752=CIRCLE('',#4771,5.5);
#1753=CIRCLE('',#4773,5.5);
#1754=CIRCLE('',#4775,3.);
#1755=CIRCLE('',#4777,3.01);
#1756=CIRCLE('',#4778,1.52);
#1757=CIRCLE('',#4779,1.52);
#1758=CIRCLE('',#4781,2.7);
#1759=CIRCLE('',#4783,5.5);
#1760=CIRCLE('',#4784,5.2);
#1761=CIRCLE('',#4787,1.05);
#1762=CIRCLE('',#4788,1.05);
#1763=CIRCLE('',#4789,1.05);
#1764=CIRCLE('',#4791,2.7);
#1765=CIRCLE('',#4793,5.2);
#1766=CIRCLE('',#4795,3.31);
#1767=CIRCLE('',#4796,3.01);
#1768=CIRCLE('',#4797,3.01);
#1769=CIRCLE('',#4799,1.52);
#1770=CIRCLE('',#4800,1.52);
#1771=CIRCLE('',#4808,0.96675);
#1772=CIRCLE('',#4815,0.739);
#1773=CIRCLE('',#4821,0.96675);
#1774=CIRCLE('',#4822,0.96675);
#1775=CIRCLE('',#4824,0.96675);
#1776=CIRCLE('',#4825,0.96675);
#1777=CIRCLE('',#4826,0.739);
#1778=CIRCLE('',#4836,0.8);
#1779=CIRCLE('',#4839,0.96675);
#1780=CIRCLE('',#4841,0.75);
#1781=CIRCLE('',#4845,1.215);
#1782=CIRCLE('',#4851,0.95825);
#1783=CIRCLE('',#4857,1.215);
#1784=CIRCLE('',#4858,1.215);
#1785=CIRCLE('',#4859,0.95825);
#1786=CIRCLE('',#4864,2.25);
#1787=CIRCLE('',#4865,2.25);
#1788=CIRCLE('',#4866,1.5);
#1789=CIRCLE('',#4868,2.25);
#1790=CIRCLE('',#4870,2.64575131106459);
#1791=CIRCLE('',#4872,2.64575131106459);
#1792=CIRCLE('',#4874,2.64575131106459);
#1793=CIRCLE('',#4876,2.64575131106459);
#1794=CIRCLE('',#4878,2.64575131106459);
#1795=CIRCLE('',#4880,2.64575131106459);
#1796=CIRCLE('',#4883,1.5);
#1797=CIRCLE('',#4884,1.5);
#1798=CIRCLE('',#4885,2.75);
#1799=CIRCLE('',#4886,1.5);
#1800=CIRCLE('',#4887,2.75);
#1801=CIRCLE('',#4889,1.05);
#1802=CIRCLE('',#4892,1.215);
#1803=CIRCLE('',#4894,2.25);
#1804=CIRCLE('',#4899,1.9);
#1805=CIRCLE('',#4900,2.24142135623731);
#1806=CIRCLE('',#4901,2.24142135623731);
#1807=CIRCLE('',#4903,2.5);
#1808=CIRCLE('',#4906,2.24142135623731);
#1809=CIRCLE('',#4907,2.24142135623731);
#1810=CIRCLE('',#4908,1.9);
#1811=CIRCLE('',#4911,2.5);
#1812=CIRCLE('',#4917,0.8);
#1813=CIRCLE('',#4918,0.56);
#1814=CIRCLE('',#4921,2.76);
#1815=CIRCLE('',#4922,3.);
#1816=CIRCLE('',#4925,0.8);
#1817=CIRCLE('',#4926,0.56);
#1818=CIRCLE('',#4929,0.8);
#1819=CIRCLE('',#4930,1.04);
#1820=CIRCLE('',#4932,3.56);
#1821=CIRCLE('',#4933,3.8);
#1822=CIRCLE('',#4935,0.8);
#1823=CIRCLE('',#4936,1.04);
#1824=CIRCLE('',#4939,0.8);
#1825=CIRCLE('',#4940,1.04);
#1826=CIRCLE('',#4943,3.);
#1827=CIRCLE('',#4944,2.76);
#1828=CIRCLE('',#4947,0.8);
#1829=CIRCLE('',#4948,1.04);
#1830=CIRCLE('',#4951,0.8);
#1831=CIRCLE('',#4952,1.04);
#1832=CIRCLE('',#4954,3.8);
#1833=CIRCLE('',#4955,3.56);
#1834=CIRCLE('',#4957,0.8);
#1835=CIRCLE('',#4958,1.04);
#1836=CIRCLE('',#4960,1.05);
#1837=CIRCLE('',#4967,2.01);
#1838=CIRCLE('',#4972,2.01);
#1839=CIRCLE('',#4974,1.05);
#1840=CIRCLE('',#4979,1.05);
#1841=CIRCLE('',#4980,1.05);
#1842=CIRCLE('',#4982,1.5);
#1843=CIRCLE('',#4984,1.5);
#1844=CIRCLE('',#4986,2.25);
#1845=CIRCLE('',#4988,2.25);
#1846=CIRCLE('',#4992,0.96675);
#1847=CIRCLE('',#5005,0.739);
#1848=CIRCLE('',#5018,0.96675);
#1849=CIRCLE('',#5019,0.96675);
#1850=CIRCLE('',#5020,0.739);
#1851=CIRCLE('',#5030,1.6);
#1852=CIRCLE('',#5038,0.8);
#1853=CIRCLE('',#5041,0.96675);
#1854=CIRCLE('',#5043,2.);
#1855=CIRCLE('',#5045,2.);
#1856=CIRCLE('',#5049,1.45);
#1857=CIRCLE('',#5050,1.25);
#1858=CIRCLE('',#5051,1.25);
#1859=CIRCLE('',#5053,1.25);
#1860=CIRCLE('',#5054,1.25);
#1861=CIRCLE('',#5056,1.8);
#1862=CIRCLE('',#5058,1.45);
#1863=CIRCLE('',#5060,1.8);
#1864=CIRCLE('',#5062,2.);
#1865=CIRCLE('',#5064,2.);
#1866=VERTEX_POINT('',#6330);
#1867=VERTEX_POINT('',#6332);
#1868=VERTEX_POINT('',#6336);
#1869=VERTEX_POINT('',#6338);
#1870=VERTEX_POINT('',#6342);
#1871=VERTEX_POINT('',#6345);
#1872=VERTEX_POINT('',#6347);
#1873=VERTEX_POINT('',#6351);
#1874=VERTEX_POINT('',#6352);
#1875=VERTEX_POINT('',#6354);
#1876=VERTEX_POINT('',#6356);
#1877=VERTEX_POINT('',#6358);
#1878=VERTEX_POINT('',#6360);
#1879=VERTEX_POINT('',#6362);
#1880=VERTEX_POINT('',#6364);
#1881=VERTEX_POINT('',#6368);
#1882=VERTEX_POINT('',#6372);
#1883=VERTEX_POINT('',#6374);
#1884=VERTEX_POINT('',#6378);
#1885=VERTEX_POINT('',#6379);
#1886=VERTEX_POINT('',#6381);
#1887=VERTEX_POINT('',#6383);
#1888=VERTEX_POINT('',#6385);
#1889=VERTEX_POINT('',#6387);
#1890=VERTEX_POINT('',#6389);
#1891=VERTEX_POINT('',#6391);
#1892=VERTEX_POINT('',#6395);
#1893=VERTEX_POINT('',#6399);
#1894=VERTEX_POINT('',#6401);
#1895=VERTEX_POINT('',#6405);
#1896=VERTEX_POINT('',#6409);
#1897=VERTEX_POINT('',#6413);
#1898=VERTEX_POINT('',#6417);
#1899=VERTEX_POINT('',#6421);
#1900=VERTEX_POINT('',#6425);
#1901=VERTEX_POINT('',#6431);
#1902=VERTEX_POINT('',#6433);
#1903=VERTEX_POINT('',#6437);
#1904=VERTEX_POINT('',#6442);
#1905=VERTEX_POINT('',#6448);
#1906=VERTEX_POINT('',#6453);
#1907=VERTEX_POINT('',#6457);
#1908=VERTEX_POINT('',#6461);
#1909=VERTEX_POINT('',#6481);
#1910=VERTEX_POINT('',#6486);
#1911=VERTEX_POINT('',#6489);
#1912=VERTEX_POINT('',#6496);
#1913=VERTEX_POINT('',#6498);
#1914=VERTEX_POINT('',#6502);
#1915=VERTEX_POINT('',#6504);
#1916=VERTEX_POINT('',#6510);
#1917=VERTEX_POINT('',#6513);
#1918=VERTEX_POINT('',#6517);
#1919=VERTEX_POINT('',#6521);
#1920=VERTEX_POINT('',#6525);
#1921=VERTEX_POINT('',#6528);
#1922=VERTEX_POINT('',#6532);
#1923=VERTEX_POINT('',#6538);
#1924=VERTEX_POINT('',#6540);
#1925=VERTEX_POINT('',#6544);
#1926=VERTEX_POINT('',#6547);
#1927=VERTEX_POINT('',#6551);
#1928=VERTEX_POINT('',#6554);
#1929=VERTEX_POINT('',#6558);
#1930=VERTEX_POINT('',#6562);
#1931=VERTEX_POINT('',#6566);
#1932=VERTEX_POINT('',#6569);
#1933=VERTEX_POINT('',#6573);
#1934=VERTEX_POINT('',#6576);
#1935=VERTEX_POINT('',#6580);
#1936=VERTEX_POINT('',#6583);
#1937=VERTEX_POINT('',#6587);
#1938=VERTEX_POINT('',#6591);
#1939=VERTEX_POINT('',#6597);
#1940=VERTEX_POINT('',#6599);
#1941=VERTEX_POINT('',#6603);
#1942=VERTEX_POINT('',#6606);
#1943=VERTEX_POINT('',#6612);
#1944=VERTEX_POINT('',#6613);
#1945=VERTEX_POINT('',#6617);
#1946=VERTEX_POINT('',#6619);
#1947=VERTEX_POINT('',#6625);
#1948=VERTEX_POINT('',#6629);
#1949=VERTEX_POINT('',#6631);
#1950=VERTEX_POINT('',#6633);
#1951=VERTEX_POINT('',#6639);
#1952=VERTEX_POINT('',#6640);
#1953=VERTEX_POINT('',#6644);
#1954=VERTEX_POINT('',#6646);
#1955=VERTEX_POINT('',#6652);
#1956=VERTEX_POINT('',#6656);
#1957=VERTEX_POINT('',#6658);
#1958=VERTEX_POINT('',#6660);
#1959=VERTEX_POINT('',#6666);
#1960=VERTEX_POINT('',#6667);
#1961=VERTEX_POINT('',#6671);
#1962=VERTEX_POINT('',#6673);
#1963=VERTEX_POINT('',#6679);
#1964=VERTEX_POINT('',#6683);
#1965=VERTEX_POINT('',#6685);
#1966=VERTEX_POINT('',#6687);
#1967=VERTEX_POINT('',#6693);
#1968=VERTEX_POINT('',#6694);
#1969=VERTEX_POINT('',#6698);
#1970=VERTEX_POINT('',#6700);
#1971=VERTEX_POINT('',#6706);
#1972=VERTEX_POINT('',#6710);
#1973=VERTEX_POINT('',#6712);
#1974=VERTEX_POINT('',#6714);
#1975=VERTEX_POINT('',#6720);
#1976=VERTEX_POINT('',#6721);
#1977=VERTEX_POINT('',#6732);
#1978=VERTEX_POINT('',#6741);
#1979=VERTEX_POINT('',#6746);
#1980=VERTEX_POINT('',#6755);
#1981=VERTEX_POINT('',#6762);
#1982=VERTEX_POINT('',#6765);
#1983=VERTEX_POINT('',#6772);
#1984=VERTEX_POINT('',#6786);
#1985=VERTEX_POINT('',#6808);
#1986=VERTEX_POINT('',#6810);
#1987=VERTEX_POINT('',#6812);
#1988=VERTEX_POINT('',#6817);
#1989=VERTEX_POINT('',#6831);
#1990=VERTEX_POINT('',#6851);
#1991=VERTEX_POINT('',#6853);
#1992=VERTEX_POINT('',#6855);
#1993=VERTEX_POINT('',#6870);
#1994=VERTEX_POINT('',#6872);
#1995=VERTEX_POINT('',#6879);
#1996=VERTEX_POINT('',#6890);
#1997=VERTEX_POINT('',#6903);
#1998=VERTEX_POINT('',#6905);
#1999=VERTEX_POINT('',#6910);
#2000=VERTEX_POINT('',#6912);
#2001=VERTEX_POINT('',#6926);
#2002=VERTEX_POINT('',#6927);
#2003=VERTEX_POINT('',#6929);
#2004=VERTEX_POINT('',#6940);
#2005=VERTEX_POINT('',#6950);
#2006=VERTEX_POINT('',#6951);
#2007=VERTEX_POINT('',#6998);
#2008=VERTEX_POINT('',#6999);
#2009=VERTEX_POINT('',#7046);
#2010=VERTEX_POINT('',#7047);
#2011=VERTEX_POINT('',#7094);
#2012=VERTEX_POINT('',#7095);
#2013=VERTEX_POINT('',#7148);
#2014=VERTEX_POINT('',#7149);
#2015=VERTEX_POINT('',#7196);
#2016=VERTEX_POINT('',#7197);
#2017=VERTEX_POINT('',#7199);
#2018=VERTEX_POINT('',#7208);
#2019=VERTEX_POINT('',#7218);
#2020=VERTEX_POINT('',#7219);
#2021=VERTEX_POINT('',#7243);
#2022=VERTEX_POINT('',#7244);
#2023=VERTEX_POINT('',#7268);
#2024=VERTEX_POINT('',#7269);
#2025=VERTEX_POINT('',#7292);
#2026=VERTEX_POINT('',#7293);
#2027=VERTEX_POINT('',#7316);
#2028=VERTEX_POINT('',#7393);
#2029=VERTEX_POINT('',#7395);
#2030=VERTEX_POINT('',#7633);
#2031=VERTEX_POINT('',#7720);
#2032=VERTEX_POINT('',#7723);
#2033=VERTEX_POINT('',#7968);
#2034=VERTEX_POINT('',#7969);
#2035=VERTEX_POINT('',#7971);
#2036=VERTEX_POINT('',#7973);
#2037=VERTEX_POINT('',#7977);
#2038=VERTEX_POINT('',#7979);
#2039=VERTEX_POINT('',#7983);
#2040=VERTEX_POINT('',#7985);
#2041=VERTEX_POINT('',#7989);
#2042=VERTEX_POINT('',#7991);
#2043=VERTEX_POINT('',#7995);
#2044=VERTEX_POINT('',#7997);
#2045=VERTEX_POINT('',#8005);
#2046=VERTEX_POINT('',#8012);
#2047=VERTEX_POINT('',#8018);
#2048=VERTEX_POINT('',#8019);
#2049=VERTEX_POINT('',#8021);
#2050=VERTEX_POINT('',#8032);
#2051=VERTEX_POINT('',#8042);
#2052=VERTEX_POINT('',#8043);
#2053=VERTEX_POINT('',#8090);
#2054=VERTEX_POINT('',#8091);
#2055=VERTEX_POINT('',#8141);
#2056=VERTEX_POINT('',#8142);
#2057=VERTEX_POINT('',#8192);
#2058=VERTEX_POINT('',#8193);
#2059=VERTEX_POINT('',#8240);
#2060=VERTEX_POINT('',#8241);
#2061=VERTEX_POINT('',#8243);
#2062=VERTEX_POINT('',#8250);
#2063=VERTEX_POINT('',#8257);
#2064=VERTEX_POINT('',#8258);
#2065=VERTEX_POINT('',#8282);
#2066=VERTEX_POINT('',#8283);
#2067=VERTEX_POINT('',#8306);
#2068=VERTEX_POINT('',#8307);
#2069=VERTEX_POINT('',#8332);
#2070=VERTEX_POINT('',#8333);
#2071=VERTEX_POINT('',#8503);
#2072=VERTEX_POINT('',#8605);
#2073=VERTEX_POINT('',#8689);
#2074=VERTEX_POINT('',#8692);
#2075=VERTEX_POINT('',#8933);
#2076=VERTEX_POINT('',#9024);
#2077=VERTEX_POINT('',#9025);
#2078=VERTEX_POINT('',#9027);
#2079=VERTEX_POINT('',#9029);
#2080=VERTEX_POINT('',#9033);
#2081=VERTEX_POINT('',#9034);
#2082=VERTEX_POINT('',#9036);
#2083=VERTEX_POINT('',#9038);
#2084=VERTEX_POINT('',#9044);
#2085=VERTEX_POINT('',#9049);
#2086=VERTEX_POINT('',#9050);
#2087=VERTEX_POINT('',#9052);
#2088=VERTEX_POINT('',#9054);
#2089=VERTEX_POINT('',#9058);
#2090=VERTEX_POINT('',#9060);
#2091=VERTEX_POINT('',#9064);
#2092=VERTEX_POINT('',#9066);
#2093=VERTEX_POINT('',#9070);
#2094=VERTEX_POINT('',#9072);
#2095=VERTEX_POINT('',#9076);
#2096=VERTEX_POINT('',#9078);
#2097=VERTEX_POINT('',#9086);
#2098=VERTEX_POINT('',#9087);
#2099=VERTEX_POINT('',#9089);
#2100=VERTEX_POINT('',#9091);
#2101=VERTEX_POINT('',#9094);
#2102=VERTEX_POINT('',#9097);
#2103=VERTEX_POINT('',#9110);
#2104=VERTEX_POINT('',#9112);
#2105=VERTEX_POINT('',#9114);
#2106=VERTEX_POINT('',#9118);
#2107=VERTEX_POINT('',#9123);
#2108=VERTEX_POINT('',#9124);
#2109=VERTEX_POINT('',#9127);
#2110=VERTEX_POINT('',#9132);
#2111=VERTEX_POINT('',#9136);
#2112=VERTEX_POINT('',#9137);
#2113=VERTEX_POINT('',#9174);
#2114=VERTEX_POINT('',#9176);
#2115=VERTEX_POINT('',#9217);
#2116=VERTEX_POINT('',#9218);
#2117=VERTEX_POINT('',#9220);
#2118=VERTEX_POINT('',#9222);
#2119=VERTEX_POINT('',#9226);
#2120=VERTEX_POINT('',#9228);
#2121=VERTEX_POINT('',#9232);
#2122=VERTEX_POINT('',#9234);
#2123=VERTEX_POINT('',#9238);
#2124=VERTEX_POINT('',#9240);
#2125=VERTEX_POINT('',#9244);
#2126=VERTEX_POINT('',#9246);
#2127=VERTEX_POINT('',#9250);
#2128=VERTEX_POINT('',#9252);
#2129=VERTEX_POINT('',#9256);
#2130=VERTEX_POINT('',#9257);
#2131=VERTEX_POINT('',#9262);
#2132=VERTEX_POINT('',#9264);
#2133=VERTEX_POINT('',#9268);
#2134=VERTEX_POINT('',#9269);
#2135=VERTEX_POINT('',#9274);
#2136=VERTEX_POINT('',#9276);
#2137=VERTEX_POINT('',#9280);
#2138=VERTEX_POINT('',#9281);
#2139=VERTEX_POINT('',#9286);
#2140=VERTEX_POINT('',#9288);
#2141=VERTEX_POINT('',#9292);
#2142=VERTEX_POINT('',#9293);
#2143=VERTEX_POINT('',#9298);
#2144=VERTEX_POINT('',#9299);
#2145=VERTEX_POINT('',#9304);
#2146=VERTEX_POINT('',#9305);
#2147=VERTEX_POINT('',#9310);
#2148=VERTEX_POINT('',#9312);
#2149=VERTEX_POINT('',#9316);
#2150=VERTEX_POINT('',#9318);
#2151=VERTEX_POINT('',#9322);
#2152=VERTEX_POINT('',#9324);
#2153=VERTEX_POINT('',#9328);
#2154=VERTEX_POINT('',#9330);
#2155=VERTEX_POINT('',#9338);
#2156=VERTEX_POINT('',#9352);
#2157=VERTEX_POINT('',#9361);
#2158=VERTEX_POINT('',#9365);
#2159=VERTEX_POINT('',#9372);
#2160=VERTEX_POINT('',#9374);
#2161=VERTEX_POINT('',#9378);
#2162=VERTEX_POINT('',#9381);
#2163=VERTEX_POINT('',#9385);
#2164=VERTEX_POINT('',#9388);
#2165=VERTEX_POINT('',#9394);
#2166=VERTEX_POINT('',#9395);
#2167=VERTEX_POINT('',#9397);
#2168=VERTEX_POINT('',#9408);
#2169=VERTEX_POINT('',#9418);
#2170=VERTEX_POINT('',#9419);
#2171=VERTEX_POINT('',#9466);
#2172=VERTEX_POINT('',#9467);
#2173=VERTEX_POINT('',#9514);
#2174=VERTEX_POINT('',#9515);
#2175=VERTEX_POINT('',#9562);
#2176=VERTEX_POINT('',#9563);
#2177=VERTEX_POINT('',#9616);
#2178=VERTEX_POINT('',#9617);
#2179=VERTEX_POINT('',#9664);
#2180=VERTEX_POINT('',#9665);
#2181=VERTEX_POINT('',#9712);
#2182=VERTEX_POINT('',#9713);
#2183=VERTEX_POINT('',#9766);
#2184=VERTEX_POINT('',#9767);
#2185=VERTEX_POINT('',#9814);
#2186=VERTEX_POINT('',#9815);
#2187=VERTEX_POINT('',#9862);
#2188=VERTEX_POINT('',#9863);
#2189=VERTEX_POINT('',#9910);
#2190=VERTEX_POINT('',#9911);
#2191=VERTEX_POINT('',#9964);
#2192=VERTEX_POINT('',#9965);
#2193=VERTEX_POINT('',#9967);
#2194=VERTEX_POINT('',#9974);
#2195=VERTEX_POINT('',#9982);
#2196=VERTEX_POINT('',#9983);
#2197=VERTEX_POINT('',#10007);
#2198=VERTEX_POINT('',#10008);
#2199=VERTEX_POINT('',#10032);
#2200=VERTEX_POINT('',#10033);
#2201=VERTEX_POINT('',#10056);
#2202=VERTEX_POINT('',#10057);
#2203=VERTEX_POINT('',#10080);
#2204=VERTEX_POINT('',#10081);
#2205=VERTEX_POINT('',#10105);
#2206=VERTEX_POINT('',#10106);
#2207=VERTEX_POINT('',#10130);
#2208=VERTEX_POINT('',#10131);
#2209=VERTEX_POINT('',#10154);
#2210=VERTEX_POINT('',#10155);
#2211=VERTEX_POINT('',#10179);
#2212=VERTEX_POINT('',#10180);
#2213=VERTEX_POINT('',#10204);
#2214=VERTEX_POINT('',#10205);
#2215=VERTEX_POINT('',#10228);
#2216=VERTEX_POINT('',#10229);
#2217=VERTEX_POINT('',#10575);
#2218=VERTEX_POINT('',#10668);
#2219=VERTEX_POINT('',#10755);
#2220=VERTEX_POINT('',#10758);
#2221=VERTEX_POINT('',#11166);
#2222=VERTEX_POINT('',#11260);
#2223=VERTEX_POINT('',#11261);
#2224=VERTEX_POINT('',#11263);
#2225=VERTEX_POINT('',#11265);
#2226=VERTEX_POINT('',#11269);
#2227=VERTEX_POINT('',#11270);
#2228=VERTEX_POINT('',#11272);
#2229=VERTEX_POINT('',#11274);
#2230=VERTEX_POINT('',#11278);
#2231=VERTEX_POINT('',#11279);
#2232=VERTEX_POINT('',#11281);
#2233=VERTEX_POINT('',#11283);
#2234=VERTEX_POINT('',#11287);
#2235=VERTEX_POINT('',#11289);
#2236=VERTEX_POINT('',#11293);
#2237=VERTEX_POINT('',#11294);
#2238=VERTEX_POINT('',#11302);
#2239=VERTEX_POINT('',#11304);
#2240=VERTEX_POINT('',#11308);
#2241=VERTEX_POINT('',#11310);
#2242=VERTEX_POINT('',#11313);
#2243=VERTEX_POINT('',#11315);
#2244=VERTEX_POINT('',#11319);
#2245=VERTEX_POINT('',#11325);
#2246=VERTEX_POINT('',#11329);
#2247=VERTEX_POINT('',#11336);
#2248=VERTEX_POINT('',#11343);
#2249=VERTEX_POINT('',#11346);
#2250=VERTEX_POINT('',#11353);
#2251=VERTEX_POINT('',#11355);
#2252=VERTEX_POINT('',#11357);
#2253=VERTEX_POINT('',#11361);
#2254=VERTEX_POINT('',#11362);
#2255=VERTEX_POINT('',#11367);
#2256=VERTEX_POINT('',#11370);
#2257=VERTEX_POINT('',#11374);
#2258=VERTEX_POINT('',#11377);
#2259=VERTEX_POINT('',#11381);
#2260=EDGE_CURVE('',#1866,#1866,#1681,.T.);
#2261=EDGE_CURVE('',#1866,#1867,#1101,.T.);
#2262=EDGE_CURVE('',#1867,#1867,#1682,.T.);
#2263=EDGE_CURVE('',#1867,#1868,#1102,.T.);
#2264=EDGE_CURVE('',#1869,#1868,#1683,.T.);
#2265=EDGE_CURVE('',#1868,#1869,#1684,.T.);
#2266=EDGE_CURVE('',#1870,#1870,#1685,.T.);
#2267=EDGE_CURVE('',#1871,#1871,#1686,.T.);
#2268=EDGE_CURVE('',#1871,#1872,#1103,.T.);
#2269=EDGE_CURVE('',#1872,#1872,#1687,.T.);
#2270=EDGE_CURVE('',#1873,#1874,#1104,.T.);
#2271=EDGE_CURVE('',#1875,#1873,#1688,.T.);
#2272=EDGE_CURVE('',#1876,#1875,#1105,.T.);
#2273=EDGE_CURVE('',#1877,#1876,#1689,.T.);
#2274=EDGE_CURVE('',#1878,#1877,#1106,.T.);
#2275=EDGE_CURVE('',#1879,#1878,#1690,.T.);
#2276=EDGE_CURVE('',#1880,#1879,#1107,.T.);
#2277=EDGE_CURVE('',#1874,#1880,#1691,.T.);
#2278=EDGE_CURVE('',#1881,#1881,#1692,.T.);
#2279=EDGE_CURVE('',#1881,#1872,#1108,.T.);
#2280=EDGE_CURVE('',#1882,#1882,#1693,.T.);
#2281=EDGE_CURVE('',#1882,#1883,#1109,.T.);
#2282=EDGE_CURVE('',#1883,#1883,#1694,.T.);
#2283=EDGE_CURVE('',#1884,#1885,#1110,.T.);
#2284=EDGE_CURVE('',#1886,#1884,#1695,.T.);
#2285=EDGE_CURVE('',#1887,#1886,#1111,.T.);
#2286=EDGE_CURVE('',#1888,#1887,#1696,.T.);
#2287=EDGE_CURVE('',#1889,#1888,#1112,.T.);
#2288=EDGE_CURVE('',#1890,#1889,#1697,.T.);
#2289=EDGE_CURVE('',#1891,#1890,#1113,.T.);
#2290=EDGE_CURVE('',#1885,#1891,#1698,.T.);
#2291=EDGE_CURVE('',#1883,#1892,#1114,.T.);
#2292=EDGE_CURVE('',#1892,#1892,#1699,.T.);
#2293=EDGE_CURVE('',#1885,#1893,#1115,.T.);
#2294=EDGE_CURVE('',#1893,#1894,#1116,.T.);
#2295=EDGE_CURVE('',#1894,#1884,#1117,.T.);
#2296=EDGE_CURVE('',#1891,#1895,#1118,.T.);
#2297=EDGE_CURVE('',#1895,#1893,#1700,.T.);
#2298=EDGE_CURVE('',#1890,#1896,#1119,.T.);
#2299=EDGE_CURVE('',#1896,#1895,#1120,.T.);
#2300=EDGE_CURVE('',#1889,#1897,#1121,.T.);
#2301=EDGE_CURVE('',#1897,#1896,#1701,.T.);
#2302=EDGE_CURVE('',#1888,#1898,#1122,.T.);
#2303=EDGE_CURVE('',#1898,#1897,#1123,.T.);
#2304=EDGE_CURVE('',#1887,#1899,#1124,.T.);
#2305=EDGE_CURVE('',#1899,#1898,#1702,.T.);
#2306=EDGE_CURVE('',#1886,#1900,#1125,.T.);
#2307=EDGE_CURVE('',#1900,#1899,#1126,.T.);
#2308=EDGE_CURVE('',#1894,#1900,#1703,.T.);
#2309=EDGE_CURVE('',#1899,#1901,#1127,.T.);
#2310=EDGE_CURVE('',#1902,#1901,#1704,.T.);
#2311=EDGE_CURVE('',#1898,#1902,#1128,.T.);
#2312=EDGE_CURVE('',#1900,#1903,#1129,.T.);
#2313=EDGE_CURVE('',#1901,#1903,#1130,.T.);
#2314=EDGE_CURVE('',#1894,#1868,#1131,.T.);
#2315=EDGE_CURVE('',#1868,#1904,#1132,.T.);
#2316=EDGE_CURVE('',#1903,#1904,#1705,.T.);
#2317=EDGE_CURVE('',#1893,#1869,#1133,.T.);
#2318=EDGE_CURVE('',#1905,#1873,#1134,.T.);
#2319=EDGE_CURVE('',#1874,#1904,#1135,.T.);
#2320=EDGE_CURVE('',#1904,#1905,#1136,.T.);
#2321=EDGE_CURVE('',#1906,#1875,#1137,.T.);
#2322=EDGE_CURVE('',#1905,#1906,#1706,.T.);
#2323=EDGE_CURVE('',#1907,#1876,#1138,.T.);
#2324=EDGE_CURVE('',#1906,#1907,#1139,.T.);
#2325=EDGE_CURVE('',#1908,#1877,#1140,.T.);
#2326=EDGE_CURVE('',#1907,#1908,#1707,.T.);
#2327=EDGE_CURVE('',#1902,#1878,#1141,.T.);
#2328=EDGE_CURVE('',#1908,#1902,#1142,.T.);
#2329=EDGE_CURVE('',#1901,#1879,#1143,.T.);
#2330=EDGE_CURVE('',#1903,#1880,#1144,.T.);
#2331=EDGE_CURVE('',#1897,#1908,#1145,.T.);
#2332=EDGE_CURVE('',#1896,#1907,#1146,.T.);
#2333=EDGE_CURVE('',#1895,#1906,#1147,.T.);
#2334=EDGE_CURVE('',#1869,#1905,#1148,.T.);
#2335=EDGE_CURVE('',#1870,#1909,#1149,.T.);
#2336=EDGE_CURVE('',#1909,#1909,#1708,.T.);
#2337=EDGE_CURVE('',#1910,#1910,#1709,.T.);
#2338=EDGE_CURVE('',#1910,#1911,#1150,.T.);
#2339=EDGE_CURVE('',#1911,#1911,#1710,.T.);
#2340=EDGE_CURVE('',#1912,#1912,#1711,.T.);
#2341=EDGE_CURVE('',#1912,#1913,#1151,.T.);
#2342=EDGE_CURVE('',#1913,#1913,#1712,.T.);
#2343=EDGE_CURVE('',#1914,#1914,#1713,.T.);
#2344=EDGE_CURVE('',#1914,#1915,#1152,.T.);
#2345=EDGE_CURVE('',#1915,#1915,#1714,.T.);
#2346=EDGE_CURVE('',#1912,#1915,#1153,.T.);
#2347=EDGE_CURVE('',#1916,#1916,#1715,.T.);
#2348=EDGE_CURVE('',#1917,#1917,#1716,.T.);
#2349=EDGE_CURVE('',#1917,#1916,#1154,.T.);
#2350=EDGE_CURVE('',#1918,#1918,#1717,.T.);
#2351=EDGE_CURVE('',#1918,#1917,#1155,.T.);
#2352=EDGE_CURVE('',#1919,#1919,#1718,.T.);
#2353=EDGE_CURVE('',#1919,#1918,#1156,.T.);
#2354=EDGE_CURVE('',#1920,#1920,#1719,.T.);
#2355=EDGE_CURVE('',#1921,#1921,#1720,.T.);
#2356=EDGE_CURVE('',#1921,#1920,#1157,.T.);
#2357=EDGE_CURVE('',#1922,#1922,#1721,.T.);
#2358=EDGE_CURVE('',#1922,#1921,#1158,.T.);
#2359=EDGE_CURVE('',#1923,#1923,#1722,.T.);
#2360=EDGE_CURVE('',#1923,#1924,#1159,.T.);
#2361=EDGE_CURVE('',#1924,#1924,#1723,.T.);
#2362=EDGE_CURVE('',#1925,#1925,#1724,.T.);
#2363=EDGE_CURVE('',#1925,#1926,#1160,.T.);
#2364=EDGE_CURVE('',#1926,#1926,#1725,.T.);
#2365=EDGE_CURVE('',#1927,#1927,#1726,.T.);
#2366=EDGE_CURVE('',#1928,#1928,#1727,.T.);
#2367=EDGE_CURVE('',#1928,#1927,#1161,.T.);
#2368=EDGE_CURVE('',#1929,#1929,#1728,.T.);
#2369=EDGE_CURVE('',#1929,#1928,#1162,.T.);
#2370=EDGE_CURVE('',#1930,#1930,#1729,.T.);
#2371=EDGE_CURVE('',#1930,#1929,#1163,.T.);
#2372=EDGE_CURVE('',#1931,#1931,#1730,.T.);
#2373=EDGE_CURVE('',#1931,#1932,#1164,.T.);
#2374=EDGE_CURVE('',#1932,#1932,#1731,.T.);
#2375=EDGE_CURVE('',#1933,#1933,#1732,.T.);
#2376=EDGE_CURVE('',#1934,#1934,#1733,.T.);
#2377=EDGE_CURVE('',#1934,#1933,#1165,.T.);
#2378=EDGE_CURVE('',#1935,#1935,#1734,.T.);
#2379=EDGE_CURVE('',#1935,#1936,#1166,.T.);
#2380=EDGE_CURVE('',#1936,#1936,#1735,.T.);
#2381=EDGE_CURVE('',#1936,#1937,#1167,.T.);
#2382=EDGE_CURVE('',#1937,#1937,#1736,.T.);
#2383=EDGE_CURVE('',#1937,#1938,#1168,.T.);
#2384=EDGE_CURVE('',#1938,#1938,#1737,.T.);
#2385=EDGE_CURVE('',#1939,#1939,#1738,.T.);
#2386=EDGE_CURVE('',#1939,#1940,#1169,.T.);
#2387=EDGE_CURVE('',#1940,#1940,#1739,.T.);
#2388=EDGE_CURVE('',#1941,#1941,#1740,.T.);
#2389=EDGE_CURVE('',#1942,#1942,#1741,.T.);
#2390=EDGE_CURVE('',#1942,#1941,#1170,.T.);
#2391=EDGE_CURVE('',#1943,#1944,#220,.F.);
#2392=EDGE_CURVE('',#1944,#1945,#1171,.T.);
#2393=EDGE_CURVE('',#1945,#1946,#221,.F.);
#2394=EDGE_CURVE('',#1946,#1943,#1172,.T.);
#2395=EDGE_CURVE('',#1947,#1944,#222,.F.);
#2396=EDGE_CURVE('',#1948,#1947,#1173,.T.);
#2397=EDGE_CURVE('',#1949,#1948,#1174,.T.);
#2398=EDGE_CURVE('',#1949,#1950,#1175,.T.);
#2399=EDGE_CURVE('',#1945,#1950,#223,.F.);
#2400=EDGE_CURVE('',#1951,#1952,#224,.F.);
#2401=EDGE_CURVE('',#1952,#1953,#1176,.T.);
#2402=EDGE_CURVE('',#1953,#1954,#225,.F.);
#2403=EDGE_CURVE('',#1954,#1951,#1177,.T.);
#2404=EDGE_CURVE('',#1955,#1952,#226,.F.);
#2405=EDGE_CURVE('',#1956,#1955,#1178,.T.);
#2406=EDGE_CURVE('',#1957,#1956,#1179,.T.);
#2407=EDGE_CURVE('',#1957,#1958,#1180,.T.);
#2408=EDGE_CURVE('',#1953,#1958,#227,.F.);
#2409=EDGE_CURVE('',#1959,#1960,#228,.F.);
#2410=EDGE_CURVE('',#1960,#1961,#1181,.T.);
#2411=EDGE_CURVE('',#1961,#1962,#229,.F.);
#2412=EDGE_CURVE('',#1962,#1959,#1182,.T.);
#2413=EDGE_CURVE('',#1963,#1960,#230,.F.);
#2414=EDGE_CURVE('',#1964,#1963,#1183,.T.);
#2415=EDGE_CURVE('',#1965,#1964,#1184,.T.);
#2416=EDGE_CURVE('',#1965,#1966,#1185,.T.);
#2417=EDGE_CURVE('',#1961,#1966,#231,.F.);
#2418=EDGE_CURVE('',#1967,#1968,#232,.F.);
#2419=EDGE_CURVE('',#1968,#1969,#1186,.T.);
#2420=EDGE_CURVE('',#1969,#1970,#233,.F.);
#2421=EDGE_CURVE('',#1970,#1967,#1187,.T.);
#2422=EDGE_CURVE('',#1971,#1968,#234,.F.);
#2423=EDGE_CURVE('',#1972,#1971,#1188,.T.);
#2424=EDGE_CURVE('',#1973,#1972,#1189,.T.);
#2425=EDGE_CURVE('',#1973,#1974,#1190,.T.);
#2426=EDGE_CURVE('',#1969,#1974,#235,.F.);
#2427=EDGE_CURVE('',#1975,#1976,#1191,.T.);
#2428=EDGE_CURVE('',#1976,#1957,#86,.T.);
#2429=EDGE_CURVE('',#1975,#1956,#87,.T.);
#2430=EDGE_CURVE('',#1976,#1977,#1742,.T.);
#2431=EDGE_CURVE('',#1977,#1948,#88,.T.);
#2432=EDGE_CURVE('',#1948,#1957,#1743,.T.);
#2433=EDGE_CURVE('',#1972,#1949,#1744,.T.);
#2434=EDGE_CURVE('',#1949,#1978,#89,.T.);
#2435=EDGE_CURVE('',#1978,#1979,#1745,.T.);
#2436=EDGE_CURVE('',#1979,#1972,#90,.T.);
#2437=EDGE_CURVE('',#1977,#1978,#1192,.T.);
#2438=EDGE_CURVE('',#1979,#1980,#1193,.T.);
#2439=EDGE_CURVE('',#1980,#1973,#91,.T.);
#2440=EDGE_CURVE('',#1964,#1981,#1746,.T.);
#2441=EDGE_CURVE('',#1981,#1973,#1747,.T.);
#2442=EDGE_CURVE('',#1980,#1982,#1748,.T.);
#2443=EDGE_CURVE('',#1982,#1964,#92,.T.);
#2444=EDGE_CURVE('',#1982,#1983,#1194,.T.);
#2445=EDGE_CURVE('',#1983,#1965,#93,.T.);
#2446=EDGE_CURVE('',#1956,#1965,#1749,.T.);
#2447=EDGE_CURVE('',#1983,#1975,#1750,.T.);
#2448=EDGE_CURVE('',#1966,#1955,#1751,.T.);
#2449=EDGE_CURVE('',#1958,#1947,#1752,.T.);
#2450=EDGE_CURVE('',#1981,#1984,#94,.T.);
#2451=EDGE_CURVE('',#1974,#1984,#1753,.T.);
#2452=EDGE_CURVE('',#1950,#1971,#1754,.T.);
#2453=EDGE_CURVE('',#1985,#1985,#1755,.T.);
#2454=EDGE_CURVE('',#1986,#1986,#1756,.T.);
#2455=EDGE_CURVE('',#1987,#1987,#1757,.T.);
#2456=EDGE_CURVE('',#1967,#1946,#1758,.T.);
#2457=EDGE_CURVE('',#1984,#1988,#95,.T.);
#2458=EDGE_CURVE('',#1988,#1963,#1759,.T.);
#2459=EDGE_CURVE('',#1959,#1970,#1760,.T.);
#2460=EDGE_CURVE('',#1988,#1989,#96,.T.);
#2461=EDGE_CURVE('',#1989,#1981,#97,.T.);
#2462=EDGE_CURVE('',#1989,#1990,#1195,.T.);
#2463=EDGE_CURVE('',#1990,#1991,#1761,.T.);
#2464=EDGE_CURVE('',#1992,#1991,#98,.T.);
#2465=EDGE_CURVE('',#1992,#1993,#1762,.T.);
#2466=EDGE_CURVE('',#1994,#1993,#99,.T.);
#2467=EDGE_CURVE('',#1995,#1994,#100,.T.);
#2468=EDGE_CURVE('',#1996,#1995,#101,.T.);
#2469=EDGE_CURVE('',#1996,#1990,#1763,.T.);
#2470=EDGE_CURVE('',#1951,#1962,#1764,.T.);
#2471=EDGE_CURVE('',#1943,#1954,#1765,.T.);
#2472=EDGE_CURVE('',#1997,#1997,#1766,.T.);
#2473=EDGE_CURVE('',#1997,#1998,#1196,.T.);
#2474=EDGE_CURVE('',#1998,#1995,#1767,.T.);
#2475=EDGE_CURVE('',#1994,#1998,#1768,.T.);
#2476=EDGE_CURVE('',#1999,#1999,#1769,.T.);
#2477=EDGE_CURVE('',#2000,#2000,#1770,.T.);
#2478=EDGE_CURVE('',#1991,#1996,#1197,.T.);
#2479=EDGE_CURVE('',#1993,#1992,#1198,.T.);
#2480=EDGE_CURVE('',#2000,#1987,#1199,.T.);
#2481=EDGE_CURVE('',#1999,#1986,#1200,.T.);
#2482=EDGE_CURVE('',#1998,#1985,#1201,.T.);
#2483=EDGE_CURVE('',#2001,#2002,#1202,.T.);
#2484=EDGE_CURVE('',#2001,#2003,#102,.T.);
#2485=EDGE_CURVE('',#2003,#2004,#1771,.T.);
#2486=EDGE_CURVE('',#2004,#2002,#103,.T.);
#2487=EDGE_CURVE('',#2005,#2006,#1203,.T.);
#2488=EDGE_CURVE('',#2005,#2001,#104,.T.);
#2489=EDGE_CURVE('',#2002,#2006,#105,.T.);
#2490=EDGE_CURVE('',#2007,#2008,#1204,.T.);
#2491=EDGE_CURVE('',#2007,#2005,#106,.T.);
#2492=EDGE_CURVE('',#2006,#2008,#107,.T.);
#2493=EDGE_CURVE('',#2009,#2010,#1205,.T.);
#2494=EDGE_CURVE('',#2009,#2007,#108,.T.);
#2495=EDGE_CURVE('',#2008,#2010,#109,.T.);
#2496=EDGE_CURVE('',#2011,#2012,#1206,.T.);
#2497=EDGE_CURVE('',#2011,#2009,#110,.T.);
#2498=EDGE_CURVE('',#2010,#2012,#111,.T.);
#2499=EDGE_CURVE('',#2013,#2014,#1207,.T.);
#2500=EDGE_CURVE('',#2013,#2011,#112,.T.);
#2501=EDGE_CURVE('',#2012,#2014,#113,.T.);
#2502=EDGE_CURVE('',#2015,#2016,#1208,.T.);
#2503=EDGE_CURVE('',#2015,#2017,#114,.T.);
#2504=EDGE_CURVE('',#2018,#2017,#1772,.T.);
#2505=EDGE_CURVE('',#2016,#2018,#115,.T.);
#2506=EDGE_CURVE('',#2019,#2020,#1209,.T.);
#2507=EDGE_CURVE('',#2019,#2015,#116,.T.);
#2508=EDGE_CURVE('',#2020,#2016,#117,.T.);
#2509=EDGE_CURVE('',#2021,#2022,#1210,.T.);
#2510=EDGE_CURVE('',#2021,#2019,#118,.T.);
#2511=EDGE_CURVE('',#2022,#2020,#119,.T.);
#2512=EDGE_CURVE('',#2023,#2024,#1211,.T.);
#2513=EDGE_CURVE('',#2023,#2021,#120,.T.);
#2514=EDGE_CURVE('',#2024,#2022,#121,.T.);
#2515=EDGE_CURVE('',#2025,#2026,#1212,.T.);
#2516=EDGE_CURVE('',#2025,#2023,#122,.T.);
#2517=EDGE_CURVE('',#2026,#2024,#123,.T.);
#2518=EDGE_CURVE('',#2017,#2027,#124,.T.);
#2519=EDGE_CURVE('',#2028,#2027,#1773,.F.);
#2520=EDGE_CURVE('',#2029,#2028,#1774,.F.);
#2521=EDGE_CURVE('',#2029,#2018,#125,.T.);
#2522=EDGE_CURVE('',#2014,#2029,#126,.T.);
#2523=EDGE_CURVE('',#2030,#2004,#127,.T.);
#2524=EDGE_CURVE('',#2030,#2026,#128,.T.);
#2525=EDGE_CURVE('',#2004,#2031,#1775,.T.);
#2526=EDGE_CURVE('',#2031,#2003,#1776,.T.);
#2527=EDGE_CURVE('',#2003,#2032,#129,.T.);
#2528=EDGE_CURVE('',#2032,#2030,#1777,.T.);
#2529=EDGE_CURVE('',#2032,#2025,#130,.T.);
#2530=EDGE_CURVE('',#2027,#2013,#131,.T.);
#2531=EDGE_CURVE('',#2033,#2034,#1213,.T.);
#2532=EDGE_CURVE('',#2033,#2035,#1214,.T.);
#2533=EDGE_CURVE('',#2035,#2036,#1215,.T.);
#2534=EDGE_CURVE('',#2034,#2036,#1216,.T.);
#2535=EDGE_CURVE('',#2037,#2033,#1217,.T.);
#2536=EDGE_CURVE('',#2037,#2038,#1218,.T.);
#2537=EDGE_CURVE('',#2038,#2035,#1219,.T.);
#2538=EDGE_CURVE('',#2039,#2037,#1220,.T.);
#2539=EDGE_CURVE('',#2039,#2040,#1221,.T.);
#2540=EDGE_CURVE('',#2040,#2038,#1222,.T.);
#2541=EDGE_CURVE('',#2041,#2039,#1223,.T.);
#2542=EDGE_CURVE('',#2041,#2042,#1224,.T.);
#2543=EDGE_CURVE('',#2042,#2040,#1225,.T.);
#2544=EDGE_CURVE('',#2043,#2041,#1226,.T.);
#2545=EDGE_CURVE('',#2043,#2044,#1227,.T.);
#2546=EDGE_CURVE('',#2044,#2042,#1228,.T.);
#2547=EDGE_CURVE('',#2034,#2043,#1229,.T.);
#2548=EDGE_CURVE('',#2036,#2044,#1230,.T.);
#2549=EDGE_CURVE('',#2045,#2045,#1778,.T.);
#2550=EDGE_CURVE('',#2031,#2045,#1231,.T.);
#2551=EDGE_CURVE('',#2027,#2029,#1779,.F.);
#2552=EDGE_CURVE('',#2046,#2046,#1780,.T.);
#2553=EDGE_CURVE('',#2046,#2028,#1232,.T.);
#2554=EDGE_CURVE('',#2047,#2048,#1233,.T.);
#2555=EDGE_CURVE('',#2047,#2049,#132,.T.);
#2556=EDGE_CURVE('',#2049,#2050,#1781,.T.);
#2557=EDGE_CURVE('',#2050,#2048,#133,.T.);
#2558=EDGE_CURVE('',#2051,#2052,#1234,.T.);
#2559=EDGE_CURVE('',#2051,#2047,#134,.T.);
#2560=EDGE_CURVE('',#2048,#2052,#135,.T.);
#2561=EDGE_CURVE('',#2053,#2054,#1235,.T.);
#2562=EDGE_CURVE('',#2053,#2051,#136,.T.);
#2563=EDGE_CURVE('',#2052,#2054,#137,.T.);
#2564=EDGE_CURVE('',#2055,#2056,#1236,.T.);
#2565=EDGE_CURVE('',#2055,#2053,#138,.T.);
#2566=EDGE_CURVE('',#2054,#2056,#139,.T.);
#2567=EDGE_CURVE('',#2057,#2058,#1237,.T.);
#2568=EDGE_CURVE('',#2057,#2055,#140,.T.);
#2569=EDGE_CURVE('',#2056,#2058,#141,.T.);
#2570=EDGE_CURVE('',#2059,#2060,#1238,.T.);
#2571=EDGE_CURVE('',#2059,#2061,#142,.T.);
#2572=EDGE_CURVE('',#2062,#2061,#1782,.T.);
#2573=EDGE_CURVE('',#2060,#2062,#143,.T.);
#2574=EDGE_CURVE('',#2063,#2064,#1239,.T.);
#2575=EDGE_CURVE('',#2063,#2059,#144,.T.);
#2576=EDGE_CURVE('',#2064,#2060,#145,.T.);
#2577=EDGE_CURVE('',#2065,#2066,#1240,.T.);
#2578=EDGE_CURVE('',#2065,#2063,#146,.T.);
#2579=EDGE_CURVE('',#2066,#2064,#147,.T.);
#2580=EDGE_CURVE('',#2067,#2068,#1241,.T.);
#2581=EDGE_CURVE('',#2067,#2065,#148,.T.);
#2582=EDGE_CURVE('',#2068,#2066,#149,.T.);
#2583=EDGE_CURVE('',#2069,#2070,#1242,.T.);
#2584=EDGE_CURVE('',#2069,#2067,#150,.T.);
#2585=EDGE_CURVE('',#2070,#2068,#151,.T.);
#2586=EDGE_CURVE('',#2071,#2062,#152,.T.);
#2587=EDGE_CURVE('',#2058,#2071,#153,.T.);
#2588=EDGE_CURVE('',#2072,#2050,#154,.T.);
#2589=EDGE_CURVE('',#2072,#2070,#155,.T.);
#2590=EDGE_CURVE('',#2050,#2073,#1783,.T.);
#2591=EDGE_CURVE('',#2073,#2049,#1784,.T.);
#2592=EDGE_CURVE('',#2049,#2074,#156,.T.);
#2593=EDGE_CURVE('',#2074,#2072,#1785,.T.);
#2594=EDGE_CURVE('',#2074,#2069,#157,.T.);
#2595=EDGE_CURVE('',#2061,#2075,#158,.T.);
#2596=EDGE_CURVE('',#2075,#2057,#159,.T.);
#2597=EDGE_CURVE('',#2076,#2077,#1243,.T.);
#2598=EDGE_CURVE('',#2078,#2076,#1244,.T.);
#2599=EDGE_CURVE('',#2079,#2078,#1245,.T.);
#2600=EDGE_CURVE('',#2077,#2079,#1246,.T.);
#2601=EDGE_CURVE('',#2080,#2081,#1247,.T.);
#2602=EDGE_CURVE('',#2082,#2080,#1248,.T.);
#2603=EDGE_CURVE('',#2083,#2082,#1249,.T.);
#2604=EDGE_CURVE('',#2081,#2083,#1250,.T.);
#2605=EDGE_CURVE('',#2079,#2081,#1786,.T.);
#2606=EDGE_CURVE('',#2083,#2077,#1787,.T.);
#2607=EDGE_CURVE('',#2084,#2084,#1788,.T.);
#2608=EDGE_CURVE('',#2078,#2080,#1789,.T.);
#2609=EDGE_CURVE('',#2085,#2086,#1790,.T.);
#2610=EDGE_CURVE('',#2085,#2087,#1251,.T.);
#2611=EDGE_CURVE('',#2087,#2088,#1252,.T.);
#2612=EDGE_CURVE('',#2086,#2088,#1253,.T.);
#2613=EDGE_CURVE('',#2086,#2089,#1791,.T.);
#2614=EDGE_CURVE('',#2088,#2090,#1254,.T.);
#2615=EDGE_CURVE('',#2089,#2090,#1255,.T.);
#2616=EDGE_CURVE('',#2089,#2091,#1792,.T.);
#2617=EDGE_CURVE('',#2090,#2092,#1256,.T.);
#2618=EDGE_CURVE('',#2091,#2092,#1257,.T.);
#2619=EDGE_CURVE('',#2091,#2093,#1793,.T.);
#2620=EDGE_CURVE('',#2092,#2094,#1258,.T.);
#2621=EDGE_CURVE('',#2093,#2094,#1259,.T.);
#2622=EDGE_CURVE('',#2095,#2085,#1794,.T.);
#2623=EDGE_CURVE('',#2095,#2096,#1260,.T.);
#2624=EDGE_CURVE('',#2096,#2087,#1261,.T.);
#2625=EDGE_CURVE('',#2093,#2095,#1795,.T.);
#2626=EDGE_CURVE('',#2094,#2096,#1262,.T.);
#2627=EDGE_CURVE('',#2097,#2098,#1796,.T.);
#2628=EDGE_CURVE('',#2099,#2097,#1797,.T.);
#2629=EDGE_CURVE('',#2099,#2100,#1798,.T.);
#2630=EDGE_CURVE('',#2098,#2099,#1799,.T.);
#2631=EDGE_CURVE('',#2101,#2098,#1800,.T.);
#2632=EDGE_CURVE('',#2102,#2102,#1801,.T.);
#2633=EDGE_CURVE('',#2073,#2102,#1263,.T.);
#2634=EDGE_CURVE('',#2075,#2071,#1802,.T.);
#2635=EDGE_CURVE('',#2082,#2076,#1803,.T.);
#2636=EDGE_CURVE('',#2097,#2084,#1264,.T.);
#2637=EDGE_CURVE('',#2103,#2103,#1804,.T.);
#2638=EDGE_CURVE('',#2103,#2104,#1265,.T.);
#2639=EDGE_CURVE('',#2104,#2105,#1805,.T.);
#2640=EDGE_CURVE('',#2105,#2104,#1806,.T.);
#2641=EDGE_CURVE('',#2105,#2106,#1266,.T.);
#2642=EDGE_CURVE('',#2106,#2106,#1807,.T.);
#2643=EDGE_CURVE('',#2107,#2108,#1808,.T.);
#2644=EDGE_CURVE('',#2108,#2107,#1809,.T.);
#2645=EDGE_CURVE('',#2107,#2109,#1267,.T.);
#2646=EDGE_CURVE('',#2109,#2109,#1810,.T.);
#2647=EDGE_CURVE('',#2110,#2110,#1811,.T.);
#2648=EDGE_CURVE('',#2110,#2108,#1268,.T.);
#2649=EDGE_CURVE('',#2111,#2112,#160,.T.);
#2650=EDGE_CURVE('',#2112,#2111,#161,.T.);
#2651=EDGE_CURVE('',#2112,#2113,#1269,.T.);
#2652=EDGE_CURVE('',#2114,#2113,#162,.T.);
#2653=EDGE_CURVE('',#2113,#2114,#163,.T.);
#2654=EDGE_CURVE('',#2106,#2110,#1270,.T.);
#2655=EDGE_CURVE('',#2115,#2116,#1271,.T.);
#2656=EDGE_CURVE('',#2116,#2117,#1272,.T.);
#2657=EDGE_CURVE('',#2117,#2118,#1273,.T.);
#2658=EDGE_CURVE('',#2118,#2115,#1274,.T.);
#2659=EDGE_CURVE('',#2115,#2119,#1812,.T.);
#2660=EDGE_CURVE('',#2119,#2120,#1275,.T.);
#2661=EDGE_CURVE('',#2120,#2116,#1813,.T.);
#2662=EDGE_CURVE('',#2119,#2121,#1276,.T.);
#2663=EDGE_CURVE('',#2121,#2122,#1277,.T.);
#2664=EDGE_CURVE('',#2122,#2120,#1278,.T.);
#2665=EDGE_CURVE('',#2121,#2123,#1814,.T.);
#2666=EDGE_CURVE('',#2123,#2124,#1279,.T.);
#2667=EDGE_CURVE('',#2124,#2122,#1815,.T.);
#2668=EDGE_CURVE('',#2123,#2125,#1280,.T.);
#2669=EDGE_CURVE('',#2125,#2126,#1281,.T.);
#2670=EDGE_CURVE('',#2126,#2124,#1282,.T.);
#2671=EDGE_CURVE('',#2125,#2127,#1816,.T.);
#2672=EDGE_CURVE('',#2127,#2128,#1283,.T.);
#2673=EDGE_CURVE('',#2128,#2126,#1817,.T.);
#2674=EDGE_CURVE('',#2129,#2130,#1284,.T.);
#2675=EDGE_CURVE('',#2130,#2128,#1285,.T.);
#2676=EDGE_CURVE('',#2127,#2129,#1286,.T.);
#2677=EDGE_CURVE('',#2129,#2131,#1818,.T.);
#2678=EDGE_CURVE('',#2131,#2132,#1287,.T.);
#2679=EDGE_CURVE('',#2132,#2130,#1819,.T.);
#2680=EDGE_CURVE('',#2133,#2134,#1288,.T.);
#2681=EDGE_CURVE('',#2134,#2132,#1820,.T.);
#2682=EDGE_CURVE('',#2131,#2133,#1821,.T.);
#2683=EDGE_CURVE('',#2133,#2135,#1822,.T.);
#2684=EDGE_CURVE('',#2135,#2136,#1289,.T.);
#2685=EDGE_CURVE('',#2136,#2134,#1823,.T.);
#2686=EDGE_CURVE('',#2137,#2138,#1290,.T.);
#2687=EDGE_CURVE('',#2138,#2136,#1291,.T.);
#2688=EDGE_CURVE('',#2135,#2137,#1292,.T.);
#2689=EDGE_CURVE('',#2137,#2139,#1824,.T.);
#2690=EDGE_CURVE('',#2139,#2140,#1293,.T.);
#2691=EDGE_CURVE('',#2140,#2138,#1825,.T.);
#2692=EDGE_CURVE('',#2141,#2142,#1294,.T.);
#2693=EDGE_CURVE('',#2142,#2140,#1295,.T.);
#2694=EDGE_CURVE('',#2139,#2141,#1296,.T.);
#2695=EDGE_CURVE('',#2143,#2144,#1297,.T.);
#2696=EDGE_CURVE('',#2144,#2142,#1826,.T.);
#2697=EDGE_CURVE('',#2141,#2143,#1827,.T.);
#2698=EDGE_CURVE('',#2145,#2146,#1298,.T.);
#2699=EDGE_CURVE('',#2146,#2144,#1299,.T.);
#2700=EDGE_CURVE('',#2143,#2145,#1300,.T.);
#2701=EDGE_CURVE('',#2145,#2147,#1828,.T.);
#2702=EDGE_CURVE('',#2147,#2148,#1301,.T.);
#2703=EDGE_CURVE('',#2148,#2146,#1829,.T.);
#2704=EDGE_CURVE('',#2147,#2149,#1302,.T.);
#2705=EDGE_CURVE('',#2149,#2150,#1303,.T.);
#2706=EDGE_CURVE('',#2150,#2148,#1304,.T.);
#2707=EDGE_CURVE('',#2149,#2151,#1830,.T.);
#2708=EDGE_CURVE('',#2151,#2152,#1305,.T.);
#2709=EDGE_CURVE('',#2152,#2150,#1831,.T.);
#2710=EDGE_CURVE('',#2151,#2153,#1832,.T.);
#2711=EDGE_CURVE('',#2153,#2154,#1306,.T.);
#2712=EDGE_CURVE('',#2154,#2152,#1833,.T.);
#2713=EDGE_CURVE('',#2153,#2118,#1834,.T.);
#2714=EDGE_CURVE('',#2117,#2154,#1835,.T.);
#2715=EDGE_CURVE('',#2125,#2119,#1307,.T.);
#2716=EDGE_CURVE('',#2155,#2155,#1836,.T.);
#2717=EDGE_CURVE('',#2133,#2151,#1308,.T.);
#2718=EDGE_CURVE('',#2149,#2135,#1309,.T.);
#2719=EDGE_CURVE('',#2153,#2131,#1310,.T.);
#2720=EDGE_CURVE('',#2115,#2127,#1311,.T.);
#2721=EDGE_CURVE('',#2129,#2118,#1312,.T.);
#2722=EDGE_CURVE('',#2144,#2122,#1313,.T.);
#2723=EDGE_CURVE('',#2156,#2156,#1837,.T.);
#2724=EDGE_CURVE('',#2142,#2124,#1314,.T.);
#2725=EDGE_CURVE('',#2137,#2147,#1315,.T.);
#2726=EDGE_CURVE('',#2145,#2139,#1316,.T.);
#2727=EDGE_CURVE('',#2156,#2157,#1317,.T.);
#2728=EDGE_CURVE('',#2157,#2157,#1838,.T.);
#2729=EDGE_CURVE('',#2155,#2158,#1318,.T.);
#2730=EDGE_CURVE('',#2158,#2158,#1839,.T.);
#2731=EDGE_CURVE('',#2159,#2159,#1840,.T.);
#2732=EDGE_CURVE('',#2159,#2160,#1319,.T.);
#2733=EDGE_CURVE('',#2160,#2160,#1841,.T.);
#2734=EDGE_CURVE('',#2161,#2161,#1842,.T.);
#2735=EDGE_CURVE('',#2162,#2162,#1843,.T.);
#2736=EDGE_CURVE('',#2162,#2161,#1320,.T.);
#2737=EDGE_CURVE('',#2163,#2163,#1844,.T.);
#2738=EDGE_CURVE('',#2164,#2164,#1845,.T.);
#2739=EDGE_CURVE('',#2164,#2163,#1321,.T.);
#2740=EDGE_CURVE('',#2165,#2166,#1322,.T.);
#2741=EDGE_CURVE('',#2165,#2167,#164,.T.);
#2742=EDGE_CURVE('',#2167,#2168,#1846,.T.);
#2743=EDGE_CURVE('',#2168,#2166,#165,.T.);
#2744=EDGE_CURVE('',#2169,#2170,#1323,.T.);
#2745=EDGE_CURVE('',#2169,#2165,#166,.T.);
#2746=EDGE_CURVE('',#2166,#2170,#167,.T.);
#2747=EDGE_CURVE('',#2171,#2172,#1324,.T.);
#2748=EDGE_CURVE('',#2171,#2169,#168,.T.);
#2749=EDGE_CURVE('',#2170,#2172,#169,.T.);
#2750=EDGE_CURVE('',#2173,#2174,#1325,.T.);
#2751=EDGE_CURVE('',#2173,#2171,#170,.T.);
#2752=EDGE_CURVE('',#2172,#2174,#171,.T.);
#2753=EDGE_CURVE('',#2175,#2176,#1326,.T.);
#2754=EDGE_CURVE('',#2175,#2173,#172,.T.);
#2755=EDGE_CURVE('',#2174,#2176,#173,.T.);
#2756=EDGE_CURVE('',#2177,#2178,#1327,.T.);
#2757=EDGE_CURVE('',#2177,#2175,#174,.T.);
#2758=EDGE_CURVE('',#2176,#2178,#175,.T.);
#2759=EDGE_CURVE('',#2179,#2180,#1328,.T.);
#2760=EDGE_CURVE('',#2179,#2177,#176,.T.);
#2761=EDGE_CURVE('',#2178,#2180,#177,.T.);
#2762=EDGE_CURVE('',#2181,#2182,#1329,.T.);
#2763=EDGE_CURVE('',#2181,#2179,#178,.T.);
#2764=EDGE_CURVE('',#2180,#2182,#179,.T.);
#2765=EDGE_CURVE('',#2183,#2184,#1330,.T.);
#2766=EDGE_CURVE('',#2183,#2181,#180,.T.);
#2767=EDGE_CURVE('',#2182,#2184,#181,.T.);
#2768=EDGE_CURVE('',#2185,#2186,#1331,.T.);
#2769=EDGE_CURVE('',#2185,#2183,#182,.T.);
#2770=EDGE_CURVE('',#2184,#2186,#183,.T.);
#2771=EDGE_CURVE('',#2187,#2188,#1332,.T.);
#2772=EDGE_CURVE('',#2187,#2185,#184,.T.);
#2773=EDGE_CURVE('',#2186,#2188,#185,.T.);
#2774=EDGE_CURVE('',#2189,#2190,#1333,.T.);
#2775=EDGE_CURVE('',#2189,#2187,#186,.T.);
#2776=EDGE_CURVE('',#2188,#2190,#187,.T.);
#2777=EDGE_CURVE('',#2191,#2192,#1334,.T.);
#2778=EDGE_CURVE('',#2191,#2193,#188,.T.);
#2779=EDGE_CURVE('',#2194,#2193,#1847,.T.);
#2780=EDGE_CURVE('',#2192,#2194,#189,.T.);
#2781=EDGE_CURVE('',#2195,#2196,#1335,.T.);
#2782=EDGE_CURVE('',#2195,#2191,#190,.T.);
#2783=EDGE_CURVE('',#2196,#2192,#191,.T.);
#2784=EDGE_CURVE('',#2197,#2198,#1336,.T.);
#2785=EDGE_CURVE('',#2197,#2195,#192,.T.);
#2786=EDGE_CURVE('',#2198,#2196,#193,.T.);
#2787=EDGE_CURVE('',#2199,#2200,#1337,.T.);
#2788=EDGE_CURVE('',#2199,#2197,#194,.T.);
#2789=EDGE_CURVE('',#2200,#2198,#195,.T.);
#2790=EDGE_CURVE('',#2201,#2202,#1338,.T.);
#2791=EDGE_CURVE('',#2201,#2199,#196,.T.);
#2792=EDGE_CURVE('',#2202,#2200,#197,.T.);
#2793=EDGE_CURVE('',#2203,#2204,#1339,.T.);
#2794=EDGE_CURVE('',#2203,#2201,#198,.T.);
#2795=EDGE_CURVE('',#2204,#2202,#199,.T.);
#2796=EDGE_CURVE('',#2205,#2206,#1340,.T.);
#2797=EDGE_CURVE('',#2205,#2203,#200,.T.);
#2798=EDGE_CURVE('',#2206,#2204,#201,.T.);
#2799=EDGE_CURVE('',#2207,#2208,#1341,.T.);
#2800=EDGE_CURVE('',#2207,#2205,#202,.T.);
#2801=EDGE_CURVE('',#2208,#2206,#203,.T.);
#2802=EDGE_CURVE('',#2209,#2210,#1342,.T.);
#2803=EDGE_CURVE('',#2209,#2207,#204,.T.);
#2804=EDGE_CURVE('',#2210,#2208,#205,.T.);
#2805=EDGE_CURVE('',#2211,#2212,#1343,.T.);
#2806=EDGE_CURVE('',#2211,#2209,#206,.T.);
#2807=EDGE_CURVE('',#2212,#2210,#207,.T.);
#2808=EDGE_CURVE('',#2213,#2214,#1344,.T.);
#2809=EDGE_CURVE('',#2213,#2211,#208,.T.);
#2810=EDGE_CURVE('',#2214,#2212,#209,.T.);
#2811=EDGE_CURVE('',#2215,#2216,#1345,.T.);
#2812=EDGE_CURVE('',#2215,#2213,#210,.T.);
#2813=EDGE_CURVE('',#2216,#2214,#211,.T.);
#2814=EDGE_CURVE('',#2217,#2194,#212,.T.);
#2815=EDGE_CURVE('',#2190,#2217,#213,.T.);
#2816=EDGE_CURVE('',#2218,#2168,#214,.T.);
#2817=EDGE_CURVE('',#2218,#2216,#215,.T.);
#2818=EDGE_CURVE('',#2168,#2219,#1848,.T.);
#2819=EDGE_CURVE('',#2219,#2167,#1849,.T.);
#2820=EDGE_CURVE('',#2167,#2220,#216,.T.);
#2821=EDGE_CURVE('',#2220,#2218,#1850,.T.);
#2822=EDGE_CURVE('',#2220,#2215,#217,.T.);
#2823=EDGE_CURVE('',#2193,#2221,#218,.T.);
#2824=EDGE_CURVE('',#2221,#2189,#219,.T.);
#2825=EDGE_CURVE('',#2222,#2223,#1346,.T.);
#2826=EDGE_CURVE('',#2224,#2222,#1347,.T.);
#2827=EDGE_CURVE('',#2224,#2225,#1348,.T.);
#2828=EDGE_CURVE('',#2225,#2223,#1349,.T.);
#2829=EDGE_CURVE('',#2226,#2227,#1350,.T.);
#2830=EDGE_CURVE('',#2226,#2228,#1351,.T.);
#2831=EDGE_CURVE('',#2229,#2228,#1352,.T.);
#2832=EDGE_CURVE('',#2227,#2229,#1353,.T.);
#2833=EDGE_CURVE('',#2230,#2231,#1354,.T.);
#2834=EDGE_CURVE('',#2232,#2230,#1355,.T.);
#2835=EDGE_CURVE('',#2232,#2233,#1356,.T.);
#2836=EDGE_CURVE('',#2233,#2231,#1357,.T.);
#2837=EDGE_CURVE('',#2234,#2232,#1358,.T.);
#2838=EDGE_CURVE('',#2234,#2235,#1359,.T.);
#2839=EDGE_CURVE('',#2235,#2233,#1360,.T.);
#2840=EDGE_CURVE('',#2236,#2237,#1361,.T.);
#2841=EDGE_CURVE('',#2236,#2235,#1362,.T.);
#2842=EDGE_CURVE('',#2237,#2234,#1363,.T.);
#2843=EDGE_CURVE('',#2229,#2224,#1364,.T.);
#2844=EDGE_CURVE('',#2228,#2225,#1365,.T.);
#2845=EDGE_CURVE('',#2231,#2238,#1366,.T.);
#2846=EDGE_CURVE('',#2239,#2238,#1367,.T.);
#2847=EDGE_CURVE('',#2230,#2239,#1368,.T.);
#2848=EDGE_CURVE('',#2240,#2240,#1851,.T.);
#2849=EDGE_CURVE('',#2239,#2241,#1369,.T.);
#2850=EDGE_CURVE('',#2241,#2227,#1370,.T.);
#2851=EDGE_CURVE('',#2222,#2242,#1371,.T.);
#2852=EDGE_CURVE('',#2242,#2243,#1372,.T.);
#2853=EDGE_CURVE('',#2243,#2237,#1373,.T.);
#2854=EDGE_CURVE('',#2241,#2244,#1374,.T.);
#2855=EDGE_CURVE('',#2244,#2226,#1375,.T.);
#2856=EDGE_CURVE('',#2238,#2244,#1376,.T.);
#2857=EDGE_CURVE('',#2243,#2245,#1377,.T.);
#2858=EDGE_CURVE('',#2245,#2236,#1378,.T.);
#2859=EDGE_CURVE('',#2242,#2246,#1379,.T.);
#2860=EDGE_CURVE('',#2246,#2245,#1380,.T.);
#2861=EDGE_CURVE('',#2223,#2246,#1381,.T.);
#2862=EDGE_CURVE('',#2247,#2247,#1852,.T.);
#2863=EDGE_CURVE('',#2219,#2247,#1382,.T.);
#2864=EDGE_CURVE('',#2221,#2217,#1853,.T.);
#2865=EDGE_CURVE('',#2248,#2248,#1854,.T.);
#2866=EDGE_CURVE('',#2249,#2249,#1855,.T.);
#2867=EDGE_CURVE('',#2249,#2248,#1383,.T.);
#2868=EDGE_CURVE('',#2240,#2249,#1384,.T.);
#2869=EDGE_CURVE('',#2250,#2250,#1856,.T.);
#2870=EDGE_CURVE('',#2250,#2251,#1385,.T.);
#2871=EDGE_CURVE('',#2251,#2252,#1857,.T.);
#2872=EDGE_CURVE('',#2252,#2251,#1858,.T.);
#2873=EDGE_CURVE('',#2253,#2254,#1859,.T.);
#2874=EDGE_CURVE('',#2254,#2253,#1860,.T.);
#2875=EDGE_CURVE('',#2254,#2252,#1386,.T.);
#2876=EDGE_CURVE('',#2255,#2255,#1861,.T.);
#2877=EDGE_CURVE('',#2253,#2256,#1387,.T.);
#2878=EDGE_CURVE('',#2256,#2256,#1862,.T.);
#2879=EDGE_CURVE('',#2257,#2257,#1863,.T.);
#2880=EDGE_CURVE('',#2258,#2258,#1864,.T.);
#2881=EDGE_CURVE('',#2258,#2255,#1388,.T.);
#2882=EDGE_CURVE('',#2259,#2259,#1865,.T.);
#2883=EDGE_CURVE('',#2259,#2258,#1389,.T.);
#2884=EDGE_CURVE('',#2257,#2259,#1390,.T.);
#2885=ORIENTED_EDGE('',*,*,#2260,.T.);
#2886=ORIENTED_EDGE('',*,*,#2261,.T.);
#2887=ORIENTED_EDGE('',*,*,#2262,.T.);
#2888=ORIENTED_EDGE('',*,*,#2261,.F.);
#2889=ORIENTED_EDGE('',*,*,#2262,.F.);
#2890=ORIENTED_EDGE('',*,*,#2263,.T.);
#2891=ORIENTED_EDGE('',*,*,#2264,.F.);
#2892=ORIENTED_EDGE('',*,*,#2265,.F.);
#2893=ORIENTED_EDGE('',*,*,#2263,.F.);
#2894=ORIENTED_EDGE('',*,*,#2260,.F.);
#2895=ORIENTED_EDGE('',*,*,#2266,.T.);
#2896=ORIENTED_EDGE('',*,*,#2267,.T.);
#2897=ORIENTED_EDGE('',*,*,#2268,.T.);
#2898=ORIENTED_EDGE('',*,*,#2269,.T.);
#2899=ORIENTED_EDGE('',*,*,#2268,.F.);
#2900=ORIENTED_EDGE('',*,*,#2270,.F.);
#2901=ORIENTED_EDGE('',*,*,#2271,.F.);
#2902=ORIENTED_EDGE('',*,*,#2272,.F.);
#2903=ORIENTED_EDGE('',*,*,#2273,.F.);
#2904=ORIENTED_EDGE('',*,*,#2274,.F.);
#2905=ORIENTED_EDGE('',*,*,#2275,.F.);
#2906=ORIENTED_EDGE('',*,*,#2276,.F.);
#2907=ORIENTED_EDGE('',*,*,#2277,.F.);
#2908=ORIENTED_EDGE('',*,*,#2267,.F.);
#2909=ORIENTED_EDGE('',*,*,#2278,.F.);
#2910=ORIENTED_EDGE('',*,*,#2279,.T.);
#2911=ORIENTED_EDGE('',*,*,#2269,.F.);
#2912=ORIENTED_EDGE('',*,*,#2279,.F.);
#2913=ORIENTED_EDGE('',*,*,#2280,.T.);
#2914=ORIENTED_EDGE('',*,*,#2281,.T.);
#2915=ORIENTED_EDGE('',*,*,#2282,.T.);
#2916=ORIENTED_EDGE('',*,*,#2281,.F.);
#2917=ORIENTED_EDGE('',*,*,#2283,.F.);
#2918=ORIENTED_EDGE('',*,*,#2284,.F.);
#2919=ORIENTED_EDGE('',*,*,#2285,.F.);
#2920=ORIENTED_EDGE('',*,*,#2286,.F.);
#2921=ORIENTED_EDGE('',*,*,#2287,.F.);
#2922=ORIENTED_EDGE('',*,*,#2288,.F.);
#2923=ORIENTED_EDGE('',*,*,#2289,.F.);
#2924=ORIENTED_EDGE('',*,*,#2290,.F.);
#2925=ORIENTED_EDGE('',*,*,#2280,.F.);
#2926=ORIENTED_EDGE('',*,*,#2282,.F.);
#2927=ORIENTED_EDGE('',*,*,#2291,.T.);
#2928=ORIENTED_EDGE('',*,*,#2292,.T.);
#2929=ORIENTED_EDGE('',*,*,#2291,.F.);
#2930=ORIENTED_EDGE('',*,*,#2293,.T.);
#2931=ORIENTED_EDGE('',*,*,#2294,.T.);
#2932=ORIENTED_EDGE('',*,*,#2295,.T.);
#2933=ORIENTED_EDGE('',*,*,#2283,.T.);
#2934=ORIENTED_EDGE('',*,*,#2296,.T.);
#2935=ORIENTED_EDGE('',*,*,#2297,.T.);
#2936=ORIENTED_EDGE('',*,*,#2293,.F.);
#2937=ORIENTED_EDGE('',*,*,#2290,.T.);
#2938=ORIENTED_EDGE('',*,*,#2298,.T.);
#2939=ORIENTED_EDGE('',*,*,#2299,.T.);
#2940=ORIENTED_EDGE('',*,*,#2296,.F.);
#2941=ORIENTED_EDGE('',*,*,#2289,.T.);
#2942=ORIENTED_EDGE('',*,*,#2300,.T.);
#2943=ORIENTED_EDGE('',*,*,#2301,.T.);
#2944=ORIENTED_EDGE('',*,*,#2298,.F.);
#2945=ORIENTED_EDGE('',*,*,#2288,.T.);
#2946=ORIENTED_EDGE('',*,*,#2302,.T.);
#2947=ORIENTED_EDGE('',*,*,#2303,.T.);
#2948=ORIENTED_EDGE('',*,*,#2300,.F.);
#2949=ORIENTED_EDGE('',*,*,#2287,.T.);
#2950=ORIENTED_EDGE('',*,*,#2304,.T.);
#2951=ORIENTED_EDGE('',*,*,#2305,.T.);
#2952=ORIENTED_EDGE('',*,*,#2302,.F.);
#2953=ORIENTED_EDGE('',*,*,#2286,.T.);
#2954=ORIENTED_EDGE('',*,*,#2306,.T.);
#2955=ORIENTED_EDGE('',*,*,#2307,.T.);
#2956=ORIENTED_EDGE('',*,*,#2304,.F.);
#2957=ORIENTED_EDGE('',*,*,#2285,.T.);
#2958=ORIENTED_EDGE('',*,*,#2295,.F.);
#2959=ORIENTED_EDGE('',*,*,#2308,.T.);
#2960=ORIENTED_EDGE('',*,*,#2306,.F.);
#2961=ORIENTED_EDGE('',*,*,#2284,.T.);
#2962=ORIENTED_EDGE('',*,*,#2305,.F.);
#2963=ORIENTED_EDGE('',*,*,#2309,.T.);
#2964=ORIENTED_EDGE('',*,*,#2310,.F.);
#2965=ORIENTED_EDGE('',*,*,#2311,.F.);
#2966=ORIENTED_EDGE('',*,*,#2307,.F.);
#2967=ORIENTED_EDGE('',*,*,#2312,.T.);
#2968=ORIENTED_EDGE('',*,*,#2313,.F.);
#2969=ORIENTED_EDGE('',*,*,#2309,.F.);
#2970=ORIENTED_EDGE('',*,*,#2308,.F.);
#2971=ORIENTED_EDGE('',*,*,#2314,.T.);
#2972=ORIENTED_EDGE('',*,*,#2315,.T.);
#2973=ORIENTED_EDGE('',*,*,#2316,.F.);
#2974=ORIENTED_EDGE('',*,*,#2312,.F.);
#2975=ORIENTED_EDGE('',*,*,#2294,.F.);
#2976=ORIENTED_EDGE('',*,*,#2317,.T.);
#2977=ORIENTED_EDGE('',*,*,#2264,.T.);
#2978=ORIENTED_EDGE('',*,*,#2314,.F.);
#2979=ORIENTED_EDGE('',*,*,#2318,.T.);
#2980=ORIENTED_EDGE('',*,*,#2270,.T.);
#2981=ORIENTED_EDGE('',*,*,#2319,.T.);
#2982=ORIENTED_EDGE('',*,*,#2320,.T.);
#2983=ORIENTED_EDGE('',*,*,#2321,.T.);
#2984=ORIENTED_EDGE('',*,*,#2271,.T.);
#2985=ORIENTED_EDGE('',*,*,#2318,.F.);
#2986=ORIENTED_EDGE('',*,*,#2322,.T.);
#2987=ORIENTED_EDGE('',*,*,#2323,.T.);
#2988=ORIENTED_EDGE('',*,*,#2272,.T.);
#2989=ORIENTED_EDGE('',*,*,#2321,.F.);
#2990=ORIENTED_EDGE('',*,*,#2324,.T.);
#2991=ORIENTED_EDGE('',*,*,#2325,.T.);
#2992=ORIENTED_EDGE('',*,*,#2273,.T.);
#2993=ORIENTED_EDGE('',*,*,#2323,.F.);
#2994=ORIENTED_EDGE('',*,*,#2326,.T.);
#2995=ORIENTED_EDGE('',*,*,#2327,.T.);
#2996=ORIENTED_EDGE('',*,*,#2274,.T.);
#2997=ORIENTED_EDGE('',*,*,#2325,.F.);
#2998=ORIENTED_EDGE('',*,*,#2328,.T.);
#2999=ORIENTED_EDGE('',*,*,#2329,.T.);
#3000=ORIENTED_EDGE('',*,*,#2275,.T.);
#3001=ORIENTED_EDGE('',*,*,#2327,.F.);
#3002=ORIENTED_EDGE('',*,*,#2310,.T.);
#3003=ORIENTED_EDGE('',*,*,#2330,.T.);
#3004=ORIENTED_EDGE('',*,*,#2276,.T.);
#3005=ORIENTED_EDGE('',*,*,#2329,.F.);
#3006=ORIENTED_EDGE('',*,*,#2313,.T.);
#3007=ORIENTED_EDGE('',*,*,#2319,.F.);
#3008=ORIENTED_EDGE('',*,*,#2277,.T.);
#3009=ORIENTED_EDGE('',*,*,#2330,.F.);
#3010=ORIENTED_EDGE('',*,*,#2316,.T.);
#3011=ORIENTED_EDGE('',*,*,#2301,.F.);
#3012=ORIENTED_EDGE('',*,*,#2331,.T.);
#3013=ORIENTED_EDGE('',*,*,#2326,.F.);
#3014=ORIENTED_EDGE('',*,*,#2332,.F.);
#3015=ORIENTED_EDGE('',*,*,#2299,.F.);
#3016=ORIENTED_EDGE('',*,*,#2332,.T.);
#3017=ORIENTED_EDGE('',*,*,#2324,.F.);
#3018=ORIENTED_EDGE('',*,*,#2333,.F.);
#3019=ORIENTED_EDGE('',*,*,#2297,.F.);
#3020=ORIENTED_EDGE('',*,*,#2333,.T.);
#3021=ORIENTED_EDGE('',*,*,#2322,.F.);
#3022=ORIENTED_EDGE('',*,*,#2334,.F.);
#3023=ORIENTED_EDGE('',*,*,#2317,.F.);
#3024=ORIENTED_EDGE('',*,*,#2320,.F.);
#3025=ORIENTED_EDGE('',*,*,#2315,.F.);
#3026=ORIENTED_EDGE('',*,*,#2265,.T.);
#3027=ORIENTED_EDGE('',*,*,#2334,.T.);
#3028=ORIENTED_EDGE('',*,*,#2266,.F.);
#3029=ORIENTED_EDGE('',*,*,#2335,.T.);
#3030=ORIENTED_EDGE('',*,*,#2336,.T.);
#3031=ORIENTED_EDGE('',*,*,#2335,.F.);
#3032=ORIENTED_EDGE('',*,*,#2336,.F.);
#3033=ORIENTED_EDGE('',*,*,#2292,.F.);
#3034=ORIENTED_EDGE('',*,*,#2337,.T.);
#3035=ORIENTED_EDGE('',*,*,#2337,.F.);
#3036=ORIENTED_EDGE('',*,*,#2338,.T.);
#3037=ORIENTED_EDGE('',*,*,#2339,.T.);
#3038=ORIENTED_EDGE('',*,*,#2338,.F.);
#3039=ORIENTED_EDGE('',*,*,#2278,.T.);
#3040=ORIENTED_EDGE('',*,*,#2339,.F.);
#3041=ORIENTED_EDGE('',*,*,#2303,.F.);
#3042=ORIENTED_EDGE('',*,*,#2311,.T.);
#3043=ORIENTED_EDGE('',*,*,#2328,.F.);
#3044=ORIENTED_EDGE('',*,*,#2331,.F.);
#3045=ORIENTED_EDGE('',*,*,#2340,.F.);
#3046=ORIENTED_EDGE('',*,*,#2341,.T.);
#3047=ORIENTED_EDGE('',*,*,#2342,.F.);
#3048=ORIENTED_EDGE('',*,*,#2341,.F.);
#3049=ORIENTED_EDGE('',*,*,#2343,.F.);
#3050=ORIENTED_EDGE('',*,*,#2344,.T.);
#3051=ORIENTED_EDGE('',*,*,#2345,.F.);
#3052=ORIENTED_EDGE('',*,*,#2344,.F.);
#3053=ORIENTED_EDGE('',*,*,#2340,.T.);
#3054=ORIENTED_EDGE('',*,*,#2346,.T.);
#3055=ORIENTED_EDGE('',*,*,#2345,.T.);
#3056=ORIENTED_EDGE('',*,*,#2346,.F.);
#3057=ORIENTED_EDGE('',*,*,#2347,.F.);
#3058=ORIENTED_EDGE('',*,*,#2343,.T.);
#3059=ORIENTED_EDGE('',*,*,#2348,.F.);
#3060=ORIENTED_EDGE('',*,*,#2349,.T.);
#3061=ORIENTED_EDGE('',*,*,#2347,.T.);
#3062=ORIENTED_EDGE('',*,*,#2349,.F.);
#3063=ORIENTED_EDGE('',*,*,#2350,.F.);
#3064=ORIENTED_EDGE('',*,*,#2351,.T.);
#3065=ORIENTED_EDGE('',*,*,#2348,.T.);
#3066=ORIENTED_EDGE('',*,*,#2351,.F.);
#3067=ORIENTED_EDGE('',*,*,#2352,.F.);
#3068=ORIENTED_EDGE('',*,*,#2353,.T.);
#3069=ORIENTED_EDGE('',*,*,#2350,.T.);
#3070=ORIENTED_EDGE('',*,*,#2353,.F.);
#3071=ORIENTED_EDGE('',*,*,#2352,.T.);
#3072=ORIENTED_EDGE('',*,*,#2354,.F.);
#3073=ORIENTED_EDGE('',*,*,#2355,.F.);
#3074=ORIENTED_EDGE('',*,*,#2356,.T.);
#3075=ORIENTED_EDGE('',*,*,#2354,.T.);
#3076=ORIENTED_EDGE('',*,*,#2356,.F.);
#3077=ORIENTED_EDGE('',*,*,#2357,.F.);
#3078=ORIENTED_EDGE('',*,*,#2358,.T.);
#3079=ORIENTED_EDGE('',*,*,#2355,.T.);
#3080=ORIENTED_EDGE('',*,*,#2358,.F.);
#3081=ORIENTED_EDGE('',*,*,#2357,.T.);
#3082=ORIENTED_EDGE('',*,*,#2342,.T.);
#3083=ORIENTED_EDGE('',*,*,#2359,.F.);
#3084=ORIENTED_EDGE('',*,*,#2360,.T.);
#3085=ORIENTED_EDGE('',*,*,#2361,.T.);
#3086=ORIENTED_EDGE('',*,*,#2360,.F.);
#3087=ORIENTED_EDGE('',*,*,#2362,.F.);
#3088=ORIENTED_EDGE('',*,*,#2359,.T.);
#3089=ORIENTED_EDGE('',*,*,#2362,.T.);
#3090=ORIENTED_EDGE('',*,*,#2363,.T.);
#3091=ORIENTED_EDGE('',*,*,#2364,.F.);
#3092=ORIENTED_EDGE('',*,*,#2363,.F.);
#3093=ORIENTED_EDGE('',*,*,#2365,.F.);
#3094=ORIENTED_EDGE('',*,*,#2364,.T.);
#3095=ORIENTED_EDGE('',*,*,#2366,.F.);
#3096=ORIENTED_EDGE('',*,*,#2367,.T.);
#3097=ORIENTED_EDGE('',*,*,#2365,.T.);
#3098=ORIENTED_EDGE('',*,*,#2367,.F.);
#3099=ORIENTED_EDGE('',*,*,#2368,.F.);
#3100=ORIENTED_EDGE('',*,*,#2369,.T.);
#3101=ORIENTED_EDGE('',*,*,#2366,.T.);
#3102=ORIENTED_EDGE('',*,*,#2369,.F.);
#3103=ORIENTED_EDGE('',*,*,#2370,.F.);
#3104=ORIENTED_EDGE('',*,*,#2371,.T.);
#3105=ORIENTED_EDGE('',*,*,#2368,.T.);
#3106=ORIENTED_EDGE('',*,*,#2371,.F.);
#3107=ORIENTED_EDGE('',*,*,#2370,.T.);
#3108=ORIENTED_EDGE('',*,*,#2372,.F.);
#3109=ORIENTED_EDGE('',*,*,#2372,.T.);
#3110=ORIENTED_EDGE('',*,*,#2373,.T.);
#3111=ORIENTED_EDGE('',*,*,#2374,.F.);
#3112=ORIENTED_EDGE('',*,*,#2373,.F.);
#3113=ORIENTED_EDGE('',*,*,#2374,.T.);
#3114=ORIENTED_EDGE('',*,*,#2375,.F.);
#3115=ORIENTED_EDGE('',*,*,#2376,.F.);
#3116=ORIENTED_EDGE('',*,*,#2377,.T.);
#3117=ORIENTED_EDGE('',*,*,#2375,.T.);
#3118=ORIENTED_EDGE('',*,*,#2377,.F.);
#3119=ORIENTED_EDGE('',*,*,#2376,.T.);
#3120=ORIENTED_EDGE('',*,*,#2378,.F.);
#3121=ORIENTED_EDGE('',*,*,#2378,.T.);
#3122=ORIENTED_EDGE('',*,*,#2379,.T.);
#3123=ORIENTED_EDGE('',*,*,#2380,.F.);
#3124=ORIENTED_EDGE('',*,*,#2379,.F.);
#3125=ORIENTED_EDGE('',*,*,#2380,.T.);
#3126=ORIENTED_EDGE('',*,*,#2381,.T.);
#3127=ORIENTED_EDGE('',*,*,#2382,.F.);
#3128=ORIENTED_EDGE('',*,*,#2381,.F.);
#3129=ORIENTED_EDGE('',*,*,#2382,.T.);
#3130=ORIENTED_EDGE('',*,*,#2383,.T.);
#3131=ORIENTED_EDGE('',*,*,#2384,.F.);
#3132=ORIENTED_EDGE('',*,*,#2383,.F.);
#3133=ORIENTED_EDGE('',*,*,#2361,.F.);
#3134=ORIENTED_EDGE('',*,*,#2384,.T.);
#3135=ORIENTED_EDGE('',*,*,#2385,.T.);
#3136=ORIENTED_EDGE('',*,*,#2386,.T.);
#3137=ORIENTED_EDGE('',*,*,#2387,.F.);
#3138=ORIENTED_EDGE('',*,*,#2386,.F.);
#3139=ORIENTED_EDGE('',*,*,#2388,.F.);
#3140=ORIENTED_EDGE('',*,*,#2387,.T.);
#3141=ORIENTED_EDGE('',*,*,#2389,.F.);
#3142=ORIENTED_EDGE('',*,*,#2390,.T.);
#3143=ORIENTED_EDGE('',*,*,#2388,.T.);
#3144=ORIENTED_EDGE('',*,*,#2390,.F.);
#3145=ORIENTED_EDGE('',*,*,#2389,.T.);
#3146=ORIENTED_EDGE('',*,*,#2385,.F.);
#3147=ORIENTED_EDGE('',*,*,#2391,.T.);
#3148=ORIENTED_EDGE('',*,*,#2392,.T.);
#3149=ORIENTED_EDGE('',*,*,#2393,.T.);
#3150=ORIENTED_EDGE('',*,*,#2394,.T.);
#3151=ORIENTED_EDGE('',*,*,#2392,.F.);
#3152=ORIENTED_EDGE('',*,*,#2395,.F.);
#3153=ORIENTED_EDGE('',*,*,#2396,.F.);
#3154=ORIENTED_EDGE('',*,*,#2397,.F.);
#3155=ORIENTED_EDGE('',*,*,#2398,.T.);
#3156=ORIENTED_EDGE('',*,*,#2399,.F.);
#3157=ORIENTED_EDGE('',*,*,#2400,.T.);
#3158=ORIENTED_EDGE('',*,*,#2401,.T.);
#3159=ORIENTED_EDGE('',*,*,#2402,.T.);
#3160=ORIENTED_EDGE('',*,*,#2403,.T.);
#3161=ORIENTED_EDGE('',*,*,#2401,.F.);
#3162=ORIENTED_EDGE('',*,*,#2404,.F.);
#3163=ORIENTED_EDGE('',*,*,#2405,.F.);
#3164=ORIENTED_EDGE('',*,*,#2406,.F.);
#3165=ORIENTED_EDGE('',*,*,#2407,.T.);
#3166=ORIENTED_EDGE('',*,*,#2408,.F.);
#3167=ORIENTED_EDGE('',*,*,#2409,.T.);
#3168=ORIENTED_EDGE('',*,*,#2410,.T.);
#3169=ORIENTED_EDGE('',*,*,#2411,.T.);
#3170=ORIENTED_EDGE('',*,*,#2412,.T.);
#3171=ORIENTED_EDGE('',*,*,#2410,.F.);
#3172=ORIENTED_EDGE('',*,*,#2413,.F.);
#3173=ORIENTED_EDGE('',*,*,#2414,.F.);
#3174=ORIENTED_EDGE('',*,*,#2415,.F.);
#3175=ORIENTED_EDGE('',*,*,#2416,.T.);
#3176=ORIENTED_EDGE('',*,*,#2417,.F.);
#3177=ORIENTED_EDGE('',*,*,#2418,.T.);
#3178=ORIENTED_EDGE('',*,*,#2419,.T.);
#3179=ORIENTED_EDGE('',*,*,#2420,.T.);
#3180=ORIENTED_EDGE('',*,*,#2421,.T.);
#3181=ORIENTED_EDGE('',*,*,#2419,.F.);
#3182=ORIENTED_EDGE('',*,*,#2422,.F.);
#3183=ORIENTED_EDGE('',*,*,#2423,.F.);
#3184=ORIENTED_EDGE('',*,*,#2424,.F.);
#3185=ORIENTED_EDGE('',*,*,#2425,.T.);
#3186=ORIENTED_EDGE('',*,*,#2426,.F.);
#3187=ORIENTED_EDGE('',*,*,#2427,.T.);
#3188=ORIENTED_EDGE('',*,*,#2428,.T.);
#3189=ORIENTED_EDGE('',*,*,#2406,.T.);
#3190=ORIENTED_EDGE('',*,*,#2429,.F.);
#3191=ORIENTED_EDGE('',*,*,#2430,.T.);
#3192=ORIENTED_EDGE('',*,*,#2431,.T.);
#3193=ORIENTED_EDGE('',*,*,#2432,.T.);
#3194=ORIENTED_EDGE('',*,*,#2428,.F.);
#3195=ORIENTED_EDGE('',*,*,#2433,.T.);
#3196=ORIENTED_EDGE('',*,*,#2434,.T.);
#3197=ORIENTED_EDGE('',*,*,#2435,.T.);
#3198=ORIENTED_EDGE('',*,*,#2436,.T.);
#3199=ORIENTED_EDGE('',*,*,#2437,.T.);
#3200=ORIENTED_EDGE('',*,*,#2434,.F.);
#3201=ORIENTED_EDGE('',*,*,#2397,.T.);
#3202=ORIENTED_EDGE('',*,*,#2431,.F.);
#3203=ORIENTED_EDGE('',*,*,#2424,.T.);
#3204=ORIENTED_EDGE('',*,*,#2436,.F.);
#3205=ORIENTED_EDGE('',*,*,#2438,.T.);
#3206=ORIENTED_EDGE('',*,*,#2439,.T.);
#3207=ORIENTED_EDGE('',*,*,#2440,.T.);
#3208=ORIENTED_EDGE('',*,*,#2441,.T.);
#3209=ORIENTED_EDGE('',*,*,#2439,.F.);
#3210=ORIENTED_EDGE('',*,*,#2442,.T.);
#3211=ORIENTED_EDGE('',*,*,#2443,.T.);
#3212=ORIENTED_EDGE('',*,*,#2415,.T.);
#3213=ORIENTED_EDGE('',*,*,#2443,.F.);
#3214=ORIENTED_EDGE('',*,*,#2444,.T.);
#3215=ORIENTED_EDGE('',*,*,#2445,.T.);
#3216=ORIENTED_EDGE('',*,*,#2446,.T.);
#3217=ORIENTED_EDGE('',*,*,#2445,.F.);
#3218=ORIENTED_EDGE('',*,*,#2447,.T.);
#3219=ORIENTED_EDGE('',*,*,#2429,.T.);
#3220=ORIENTED_EDGE('',*,*,#2446,.F.);
#3221=ORIENTED_EDGE('',*,*,#2405,.T.);
#3222=ORIENTED_EDGE('',*,*,#2448,.F.);
#3223=ORIENTED_EDGE('',*,*,#2416,.F.);
#3224=ORIENTED_EDGE('',*,*,#2432,.F.);
#3225=ORIENTED_EDGE('',*,*,#2396,.T.);
#3226=ORIENTED_EDGE('',*,*,#2449,.F.);
#3227=ORIENTED_EDGE('',*,*,#2407,.F.);
#3228=ORIENTED_EDGE('',*,*,#2441,.F.);
#3229=ORIENTED_EDGE('',*,*,#2450,.T.);
#3230=ORIENTED_EDGE('',*,*,#2451,.F.);
#3231=ORIENTED_EDGE('',*,*,#2425,.F.);
#3232=ORIENTED_EDGE('',*,*,#2433,.F.);
#3233=ORIENTED_EDGE('',*,*,#2423,.T.);
#3234=ORIENTED_EDGE('',*,*,#2452,.F.);
#3235=ORIENTED_EDGE('',*,*,#2398,.F.);
#3236=ORIENTED_EDGE('',*,*,#2435,.F.);
#3237=ORIENTED_EDGE('',*,*,#2437,.F.);
#3238=ORIENTED_EDGE('',*,*,#2430,.F.);
#3239=ORIENTED_EDGE('',*,*,#2427,.F.);
#3240=ORIENTED_EDGE('',*,*,#2447,.F.);
#3241=ORIENTED_EDGE('',*,*,#2444,.F.);
#3242=ORIENTED_EDGE('',*,*,#2442,.F.);
#3243=ORIENTED_EDGE('',*,*,#2438,.F.);
#3244=ORIENTED_EDGE('',*,*,#2453,.T.);
#3245=ORIENTED_EDGE('',*,*,#2454,.T.);
#3246=ORIENTED_EDGE('',*,*,#2455,.T.);
#3247=ORIENTED_EDGE('',*,*,#2399,.T.);
#3248=ORIENTED_EDGE('',*,*,#2452,.T.);
#3249=ORIENTED_EDGE('',*,*,#2422,.T.);
#3250=ORIENTED_EDGE('',*,*,#2418,.F.);
#3251=ORIENTED_EDGE('',*,*,#2456,.T.);
#3252=ORIENTED_EDGE('',*,*,#2393,.F.);
#3253=ORIENTED_EDGE('',*,*,#2457,.T.);
#3254=ORIENTED_EDGE('',*,*,#2458,.T.);
#3255=ORIENTED_EDGE('',*,*,#2413,.T.);
#3256=ORIENTED_EDGE('',*,*,#2409,.F.);
#3257=ORIENTED_EDGE('',*,*,#2459,.T.);
#3258=ORIENTED_EDGE('',*,*,#2420,.F.);
#3259=ORIENTED_EDGE('',*,*,#2426,.T.);
#3260=ORIENTED_EDGE('',*,*,#2451,.T.);
#3261=ORIENTED_EDGE('',*,*,#2440,.F.);
#3262=ORIENTED_EDGE('',*,*,#2414,.T.);
#3263=ORIENTED_EDGE('',*,*,#2458,.F.);
#3264=ORIENTED_EDGE('',*,*,#2460,.T.);
#3265=ORIENTED_EDGE('',*,*,#2461,.T.);
#3266=ORIENTED_EDGE('',*,*,#2457,.F.);
#3267=ORIENTED_EDGE('',*,*,#2450,.F.);
#3268=ORIENTED_EDGE('',*,*,#2461,.F.);
#3269=ORIENTED_EDGE('',*,*,#2462,.T.);
#3270=ORIENTED_EDGE('',*,*,#2463,.T.);
#3271=ORIENTED_EDGE('',*,*,#2464,.F.);
#3272=ORIENTED_EDGE('',*,*,#2465,.T.);
#3273=ORIENTED_EDGE('',*,*,#2466,.F.);
#3274=ORIENTED_EDGE('',*,*,#2467,.F.);
#3275=ORIENTED_EDGE('',*,*,#2468,.F.);
#3276=ORIENTED_EDGE('',*,*,#2469,.T.);
#3277=ORIENTED_EDGE('',*,*,#2462,.F.);
#3278=ORIENTED_EDGE('',*,*,#2460,.F.);
#3279=ORIENTED_EDGE('',*,*,#2417,.T.);
#3280=ORIENTED_EDGE('',*,*,#2448,.T.);
#3281=ORIENTED_EDGE('',*,*,#2404,.T.);
#3282=ORIENTED_EDGE('',*,*,#2400,.F.);
#3283=ORIENTED_EDGE('',*,*,#2470,.T.);
#3284=ORIENTED_EDGE('',*,*,#2411,.F.);
#3285=ORIENTED_EDGE('',*,*,#2408,.T.);
#3286=ORIENTED_EDGE('',*,*,#2449,.T.);
#3287=ORIENTED_EDGE('',*,*,#2395,.T.);
#3288=ORIENTED_EDGE('',*,*,#2391,.F.);
#3289=ORIENTED_EDGE('',*,*,#2471,.T.);
#3290=ORIENTED_EDGE('',*,*,#2402,.F.);
#3291=ORIENTED_EDGE('',*,*,#2472,.T.);
#3292=ORIENTED_EDGE('',*,*,#2473,.T.);
#3293=ORIENTED_EDGE('',*,*,#2474,.T.);
#3294=ORIENTED_EDGE('',*,*,#2467,.T.);
#3295=ORIENTED_EDGE('',*,*,#2475,.T.);
#3296=ORIENTED_EDGE('',*,*,#2473,.F.);
#3297=ORIENTED_EDGE('',*,*,#2456,.F.);
#3298=ORIENTED_EDGE('',*,*,#2421,.F.);
#3299=ORIENTED_EDGE('',*,*,#2459,.F.);
#3300=ORIENTED_EDGE('',*,*,#2412,.F.);
#3301=ORIENTED_EDGE('',*,*,#2470,.F.);
#3302=ORIENTED_EDGE('',*,*,#2403,.F.);
#3303=ORIENTED_EDGE('',*,*,#2471,.F.);
#3304=ORIENTED_EDGE('',*,*,#2394,.F.);
#3305=ORIENTED_EDGE('',*,*,#2476,.T.);
#3306=ORIENTED_EDGE('',*,*,#2477,.T.);
#3307=ORIENTED_EDGE('',*,*,#2472,.F.);
#3308=ORIENTED_EDGE('',*,*,#2478,.F.);
#3309=ORIENTED_EDGE('',*,*,#2463,.F.);
#3310=ORIENTED_EDGE('',*,*,#2469,.F.);
#3311=ORIENTED_EDGE('',*,*,#2479,.F.);
#3312=ORIENTED_EDGE('',*,*,#2465,.F.);
#3313=ORIENTED_EDGE('',*,*,#2477,.F.);
#3314=ORIENTED_EDGE('',*,*,#2480,.T.);
#3315=ORIENTED_EDGE('',*,*,#2455,.F.);
#3316=ORIENTED_EDGE('',*,*,#2480,.F.);
#3317=ORIENTED_EDGE('',*,*,#2476,.F.);
#3318=ORIENTED_EDGE('',*,*,#2481,.T.);
#3319=ORIENTED_EDGE('',*,*,#2454,.F.);
#3320=ORIENTED_EDGE('',*,*,#2481,.F.);
#3321=ORIENTED_EDGE('',*,*,#2475,.F.);
#3322=ORIENTED_EDGE('',*,*,#2466,.T.);
#3323=ORIENTED_EDGE('',*,*,#2479,.T.);
#3324=ORIENTED_EDGE('',*,*,#2464,.T.);
#3325=ORIENTED_EDGE('',*,*,#2478,.T.);
#3326=ORIENTED_EDGE('',*,*,#2468,.T.);
#3327=ORIENTED_EDGE('',*,*,#2474,.F.);
#3328=ORIENTED_EDGE('',*,*,#2482,.T.);
#3329=ORIENTED_EDGE('',*,*,#2453,.F.);
#3330=ORIENTED_EDGE('',*,*,#2482,.F.);
#3331=ORIENTED_EDGE('',*,*,#2483,.F.);
#3332=ORIENTED_EDGE('',*,*,#2484,.T.);
#3333=ORIENTED_EDGE('',*,*,#2485,.T.);
#3334=ORIENTED_EDGE('',*,*,#2486,.T.);
#3335=ORIENTED_EDGE('',*,*,#2487,.F.);
#3336=ORIENTED_EDGE('',*,*,#2488,.T.);
#3337=ORIENTED_EDGE('',*,*,#2483,.T.);
#3338=ORIENTED_EDGE('',*,*,#2489,.T.);
#3339=ORIENTED_EDGE('',*,*,#2490,.F.);
#3340=ORIENTED_EDGE('',*,*,#2491,.T.);
#3341=ORIENTED_EDGE('',*,*,#2487,.T.);
#3342=ORIENTED_EDGE('',*,*,#2492,.T.);
#3343=ORIENTED_EDGE('',*,*,#2493,.F.);
#3344=ORIENTED_EDGE('',*,*,#2494,.T.);
#3345=ORIENTED_EDGE('',*,*,#2490,.T.);
#3346=ORIENTED_EDGE('',*,*,#2495,.T.);
#3347=ORIENTED_EDGE('',*,*,#2496,.F.);
#3348=ORIENTED_EDGE('',*,*,#2497,.T.);
#3349=ORIENTED_EDGE('',*,*,#2493,.T.);
#3350=ORIENTED_EDGE('',*,*,#2498,.T.);
#3351=ORIENTED_EDGE('',*,*,#2499,.F.);
#3352=ORIENTED_EDGE('',*,*,#2500,.T.);
#3353=ORIENTED_EDGE('',*,*,#2496,.T.);
#3354=ORIENTED_EDGE('',*,*,#2501,.T.);
#3355=ORIENTED_EDGE('',*,*,#2502,.F.);
#3356=ORIENTED_EDGE('',*,*,#2503,.T.);
#3357=ORIENTED_EDGE('',*,*,#2504,.F.);
#3358=ORIENTED_EDGE('',*,*,#2505,.F.);
#3359=ORIENTED_EDGE('',*,*,#2506,.F.);
#3360=ORIENTED_EDGE('',*,*,#2507,.T.);
#3361=ORIENTED_EDGE('',*,*,#2502,.T.);
#3362=ORIENTED_EDGE('',*,*,#2508,.F.);
#3363=ORIENTED_EDGE('',*,*,#2509,.F.);
#3364=ORIENTED_EDGE('',*,*,#2510,.T.);
#3365=ORIENTED_EDGE('',*,*,#2506,.T.);
#3366=ORIENTED_EDGE('',*,*,#2511,.F.);
#3367=ORIENTED_EDGE('',*,*,#2512,.F.);
#3368=ORIENTED_EDGE('',*,*,#2513,.T.);
#3369=ORIENTED_EDGE('',*,*,#2509,.T.);
#3370=ORIENTED_EDGE('',*,*,#2514,.F.);
#3371=ORIENTED_EDGE('',*,*,#2515,.F.);
#3372=ORIENTED_EDGE('',*,*,#2516,.T.);
#3373=ORIENTED_EDGE('',*,*,#2512,.T.);
#3374=ORIENTED_EDGE('',*,*,#2517,.F.);
#3375=ORIENTED_EDGE('',*,*,#2504,.T.);
#3376=ORIENTED_EDGE('',*,*,#2518,.T.);
#3377=ORIENTED_EDGE('',*,*,#2519,.F.);
#3378=ORIENTED_EDGE('',*,*,#2520,.F.);
#3379=ORIENTED_EDGE('',*,*,#2521,.T.);
#3380=ORIENTED_EDGE('',*,*,#2521,.F.);
#3381=ORIENTED_EDGE('',*,*,#2522,.F.);
#3382=ORIENTED_EDGE('',*,*,#2501,.F.);
#3383=ORIENTED_EDGE('',*,*,#2498,.F.);
#3384=ORIENTED_EDGE('',*,*,#2495,.F.);
#3385=ORIENTED_EDGE('',*,*,#2492,.F.);
#3386=ORIENTED_EDGE('',*,*,#2489,.F.);
#3387=ORIENTED_EDGE('',*,*,#2486,.F.);
#3388=ORIENTED_EDGE('',*,*,#2523,.F.);
#3389=ORIENTED_EDGE('',*,*,#2524,.T.);
#3390=ORIENTED_EDGE('',*,*,#2517,.T.);
#3391=ORIENTED_EDGE('',*,*,#2514,.T.);
#3392=ORIENTED_EDGE('',*,*,#2511,.T.);
#3393=ORIENTED_EDGE('',*,*,#2508,.T.);
#3394=ORIENTED_EDGE('',*,*,#2505,.T.);
#3395=ORIENTED_EDGE('',*,*,#2525,.T.);
#3396=ORIENTED_EDGE('',*,*,#2526,.T.);
#3397=ORIENTED_EDGE('',*,*,#2527,.T.);
#3398=ORIENTED_EDGE('',*,*,#2528,.T.);
#3399=ORIENTED_EDGE('',*,*,#2523,.T.);
#3400=ORIENTED_EDGE('',*,*,#2515,.T.);
#3401=ORIENTED_EDGE('',*,*,#2524,.F.);
#3402=ORIENTED_EDGE('',*,*,#2528,.F.);
#3403=ORIENTED_EDGE('',*,*,#2529,.T.);
#3404=ORIENTED_EDGE('',*,*,#2518,.F.);
#3405=ORIENTED_EDGE('',*,*,#2503,.F.);
#3406=ORIENTED_EDGE('',*,*,#2507,.F.);
#3407=ORIENTED_EDGE('',*,*,#2510,.F.);
#3408=ORIENTED_EDGE('',*,*,#2513,.F.);
#3409=ORIENTED_EDGE('',*,*,#2516,.F.);
#3410=ORIENTED_EDGE('',*,*,#2529,.F.);
#3411=ORIENTED_EDGE('',*,*,#2527,.F.);
#3412=ORIENTED_EDGE('',*,*,#2484,.F.);
#3413=ORIENTED_EDGE('',*,*,#2488,.F.);
#3414=ORIENTED_EDGE('',*,*,#2491,.F.);
#3415=ORIENTED_EDGE('',*,*,#2494,.F.);
#3416=ORIENTED_EDGE('',*,*,#2497,.F.);
#3417=ORIENTED_EDGE('',*,*,#2500,.F.);
#3418=ORIENTED_EDGE('',*,*,#2530,.F.);
#3419=ORIENTED_EDGE('',*,*,#2531,.F.);
#3420=ORIENTED_EDGE('',*,*,#2532,.T.);
#3421=ORIENTED_EDGE('',*,*,#2533,.T.);
#3422=ORIENTED_EDGE('',*,*,#2534,.F.);
#3423=ORIENTED_EDGE('',*,*,#2535,.F.);
#3424=ORIENTED_EDGE('',*,*,#2536,.T.);
#3425=ORIENTED_EDGE('',*,*,#2537,.T.);
#3426=ORIENTED_EDGE('',*,*,#2532,.F.);
#3427=ORIENTED_EDGE('',*,*,#2538,.F.);
#3428=ORIENTED_EDGE('',*,*,#2539,.T.);
#3429=ORIENTED_EDGE('',*,*,#2540,.T.);
#3430=ORIENTED_EDGE('',*,*,#2536,.F.);
#3431=ORIENTED_EDGE('',*,*,#2541,.F.);
#3432=ORIENTED_EDGE('',*,*,#2542,.T.);
#3433=ORIENTED_EDGE('',*,*,#2543,.T.);
#3434=ORIENTED_EDGE('',*,*,#2539,.F.);
#3435=ORIENTED_EDGE('',*,*,#2544,.F.);
#3436=ORIENTED_EDGE('',*,*,#2545,.T.);
#3437=ORIENTED_EDGE('',*,*,#2546,.T.);
#3438=ORIENTED_EDGE('',*,*,#2542,.F.);
#3439=ORIENTED_EDGE('',*,*,#2547,.F.);
#3440=ORIENTED_EDGE('',*,*,#2534,.T.);
#3441=ORIENTED_EDGE('',*,*,#2548,.T.);
#3442=ORIENTED_EDGE('',*,*,#2545,.F.);
#3443=ORIENTED_EDGE('',*,*,#2548,.F.);
#3444=ORIENTED_EDGE('',*,*,#2533,.F.);
#3445=ORIENTED_EDGE('',*,*,#2537,.F.);
#3446=ORIENTED_EDGE('',*,*,#2540,.F.);
#3447=ORIENTED_EDGE('',*,*,#2543,.F.);
#3448=ORIENTED_EDGE('',*,*,#2546,.F.);
#3449=ORIENTED_EDGE('',*,*,#2549,.F.);
#3450=ORIENTED_EDGE('',*,*,#2531,.T.);
#3451=ORIENTED_EDGE('',*,*,#2547,.T.);
#3452=ORIENTED_EDGE('',*,*,#2544,.T.);
#3453=ORIENTED_EDGE('',*,*,#2541,.T.);
#3454=ORIENTED_EDGE('',*,*,#2538,.T.);
#3455=ORIENTED_EDGE('',*,*,#2535,.T.);
#3456=ORIENTED_EDGE('',*,*,#2525,.F.);
#3457=ORIENTED_EDGE('',*,*,#2485,.F.);
#3458=ORIENTED_EDGE('',*,*,#2526,.F.);
#3459=ORIENTED_EDGE('',*,*,#2550,.T.);
#3460=ORIENTED_EDGE('',*,*,#2549,.T.);
#3461=ORIENTED_EDGE('',*,*,#2550,.F.);
#3462=ORIENTED_EDGE('',*,*,#2499,.T.);
#3463=ORIENTED_EDGE('',*,*,#2522,.T.);
#3464=ORIENTED_EDGE('',*,*,#2551,.F.);
#3465=ORIENTED_EDGE('',*,*,#2530,.T.);
#3466=ORIENTED_EDGE('',*,*,#2552,.F.);
#3467=ORIENTED_EDGE('',*,*,#2553,.T.);
#3468=ORIENTED_EDGE('',*,*,#2519,.T.);
#3469=ORIENTED_EDGE('',*,*,#2551,.T.);
#3470=ORIENTED_EDGE('',*,*,#2520,.T.);
#3471=ORIENTED_EDGE('',*,*,#2553,.F.);
#3472=ORIENTED_EDGE('',*,*,#2552,.T.);
#3473=ORIENTED_EDGE('',*,*,#2554,.F.);
#3474=ORIENTED_EDGE('',*,*,#2555,.T.);
#3475=ORIENTED_EDGE('',*,*,#2556,.T.);
#3476=ORIENTED_EDGE('',*,*,#2557,.T.);
#3477=ORIENTED_EDGE('',*,*,#2558,.F.);
#3478=ORIENTED_EDGE('',*,*,#2559,.T.);
#3479=ORIENTED_EDGE('',*,*,#2554,.T.);
#3480=ORIENTED_EDGE('',*,*,#2560,.T.);
#3481=ORIENTED_EDGE('',*,*,#2561,.F.);
#3482=ORIENTED_EDGE('',*,*,#2562,.T.);
#3483=ORIENTED_EDGE('',*,*,#2558,.T.);
#3484=ORIENTED_EDGE('',*,*,#2563,.T.);
#3485=ORIENTED_EDGE('',*,*,#2564,.F.);
#3486=ORIENTED_EDGE('',*,*,#2565,.T.);
#3487=ORIENTED_EDGE('',*,*,#2561,.T.);
#3488=ORIENTED_EDGE('',*,*,#2566,.T.);
#3489=ORIENTED_EDGE('',*,*,#2567,.F.);
#3490=ORIENTED_EDGE('',*,*,#2568,.T.);
#3491=ORIENTED_EDGE('',*,*,#2564,.T.);
#3492=ORIENTED_EDGE('',*,*,#2569,.T.);
#3493=ORIENTED_EDGE('',*,*,#2570,.F.);
#3494=ORIENTED_EDGE('',*,*,#2571,.T.);
#3495=ORIENTED_EDGE('',*,*,#2572,.F.);
#3496=ORIENTED_EDGE('',*,*,#2573,.F.);
#3497=ORIENTED_EDGE('',*,*,#2574,.F.);
#3498=ORIENTED_EDGE('',*,*,#2575,.T.);
#3499=ORIENTED_EDGE('',*,*,#2570,.T.);
#3500=ORIENTED_EDGE('',*,*,#2576,.F.);
#3501=ORIENTED_EDGE('',*,*,#2577,.F.);
#3502=ORIENTED_EDGE('',*,*,#2578,.T.);
#3503=ORIENTED_EDGE('',*,*,#2574,.T.);
#3504=ORIENTED_EDGE('',*,*,#2579,.F.);
#3505=ORIENTED_EDGE('',*,*,#2580,.F.);
#3506=ORIENTED_EDGE('',*,*,#2581,.T.);
#3507=ORIENTED_EDGE('',*,*,#2577,.T.);
#3508=ORIENTED_EDGE('',*,*,#2582,.F.);
#3509=ORIENTED_EDGE('',*,*,#2583,.F.);
#3510=ORIENTED_EDGE('',*,*,#2584,.T.);
#3511=ORIENTED_EDGE('',*,*,#2580,.T.);
#3512=ORIENTED_EDGE('',*,*,#2585,.F.);
#3513=ORIENTED_EDGE('',*,*,#2586,.F.);
#3514=ORIENTED_EDGE('',*,*,#2587,.F.);
#3515=ORIENTED_EDGE('',*,*,#2569,.F.);
#3516=ORIENTED_EDGE('',*,*,#2566,.F.);
#3517=ORIENTED_EDGE('',*,*,#2563,.F.);
#3518=ORIENTED_EDGE('',*,*,#2560,.F.);
#3519=ORIENTED_EDGE('',*,*,#2557,.F.);
#3520=ORIENTED_EDGE('',*,*,#2588,.F.);
#3521=ORIENTED_EDGE('',*,*,#2589,.T.);
#3522=ORIENTED_EDGE('',*,*,#2585,.T.);
#3523=ORIENTED_EDGE('',*,*,#2582,.T.);
#3524=ORIENTED_EDGE('',*,*,#2579,.T.);
#3525=ORIENTED_EDGE('',*,*,#2576,.T.);
#3526=ORIENTED_EDGE('',*,*,#2573,.T.);
#3527=ORIENTED_EDGE('',*,*,#2590,.T.);
#3528=ORIENTED_EDGE('',*,*,#2591,.T.);
#3529=ORIENTED_EDGE('',*,*,#2592,.T.);
#3530=ORIENTED_EDGE('',*,*,#2593,.T.);
#3531=ORIENTED_EDGE('',*,*,#2588,.T.);
#3532=ORIENTED_EDGE('',*,*,#2583,.T.);
#3533=ORIENTED_EDGE('',*,*,#2589,.F.);
#3534=ORIENTED_EDGE('',*,*,#2593,.F.);
#3535=ORIENTED_EDGE('',*,*,#2594,.T.);
#3536=ORIENTED_EDGE('',*,*,#2595,.F.);
#3537=ORIENTED_EDGE('',*,*,#2571,.F.);
#3538=ORIENTED_EDGE('',*,*,#2575,.F.);
#3539=ORIENTED_EDGE('',*,*,#2578,.F.);
#3540=ORIENTED_EDGE('',*,*,#2581,.F.);
#3541=ORIENTED_EDGE('',*,*,#2584,.F.);
#3542=ORIENTED_EDGE('',*,*,#2594,.F.);
#3543=ORIENTED_EDGE('',*,*,#2592,.F.);
#3544=ORIENTED_EDGE('',*,*,#2555,.F.);
#3545=ORIENTED_EDGE('',*,*,#2559,.F.);
#3546=ORIENTED_EDGE('',*,*,#2562,.F.);
#3547=ORIENTED_EDGE('',*,*,#2565,.F.);
#3548=ORIENTED_EDGE('',*,*,#2568,.F.);
#3549=ORIENTED_EDGE('',*,*,#2596,.F.);
#3550=ORIENTED_EDGE('',*,*,#2597,.F.);
#3551=ORIENTED_EDGE('',*,*,#2598,.F.);
#3552=ORIENTED_EDGE('',*,*,#2599,.F.);
#3553=ORIENTED_EDGE('',*,*,#2600,.F.);
#3554=ORIENTED_EDGE('',*,*,#2601,.F.);
#3555=ORIENTED_EDGE('',*,*,#2602,.F.);
#3556=ORIENTED_EDGE('',*,*,#2603,.F.);
#3557=ORIENTED_EDGE('',*,*,#2604,.F.);
#3558=ORIENTED_EDGE('',*,*,#2600,.T.);
#3559=ORIENTED_EDGE('',*,*,#2605,.T.);
#3560=ORIENTED_EDGE('',*,*,#2604,.T.);
#3561=ORIENTED_EDGE('',*,*,#2606,.T.);
#3562=ORIENTED_EDGE('',*,*,#2607,.F.);
#3563=ORIENTED_EDGE('',*,*,#2599,.T.);
#3564=ORIENTED_EDGE('',*,*,#2608,.T.);
#3565=ORIENTED_EDGE('',*,*,#2601,.T.);
#3566=ORIENTED_EDGE('',*,*,#2605,.F.);
#3567=ORIENTED_EDGE('',*,*,#2609,.F.);
#3568=ORIENTED_EDGE('',*,*,#2610,.T.);
#3569=ORIENTED_EDGE('',*,*,#2611,.T.);
#3570=ORIENTED_EDGE('',*,*,#2612,.F.);
#3571=ORIENTED_EDGE('',*,*,#2613,.F.);
#3572=ORIENTED_EDGE('',*,*,#2612,.T.);
#3573=ORIENTED_EDGE('',*,*,#2614,.T.);
#3574=ORIENTED_EDGE('',*,*,#2615,.F.);
#3575=ORIENTED_EDGE('',*,*,#2616,.F.);
#3576=ORIENTED_EDGE('',*,*,#2615,.T.);
#3577=ORIENTED_EDGE('',*,*,#2617,.T.);
#3578=ORIENTED_EDGE('',*,*,#2618,.F.);
#3579=ORIENTED_EDGE('',*,*,#2619,.F.);
#3580=ORIENTED_EDGE('',*,*,#2618,.T.);
#3581=ORIENTED_EDGE('',*,*,#2620,.T.);
#3582=ORIENTED_EDGE('',*,*,#2621,.F.);
#3583=ORIENTED_EDGE('',*,*,#2622,.F.);
#3584=ORIENTED_EDGE('',*,*,#2623,.T.);
#3585=ORIENTED_EDGE('',*,*,#2624,.T.);
#3586=ORIENTED_EDGE('',*,*,#2610,.F.);
#3587=ORIENTED_EDGE('',*,*,#2625,.F.);
#3588=ORIENTED_EDGE('',*,*,#2621,.T.);
#3589=ORIENTED_EDGE('',*,*,#2626,.T.);
#3590=ORIENTED_EDGE('',*,*,#2623,.F.);
#3591=ORIENTED_EDGE('',*,*,#2626,.F.);
#3592=ORIENTED_EDGE('',*,*,#2620,.F.);
#3593=ORIENTED_EDGE('',*,*,#2617,.F.);
#3594=ORIENTED_EDGE('',*,*,#2614,.F.);
#3595=ORIENTED_EDGE('',*,*,#2611,.F.);
#3596=ORIENTED_EDGE('',*,*,#2624,.F.);
#3597=ORIENTED_EDGE('',*,*,#2627,.F.);
#3598=ORIENTED_EDGE('',*,*,#2628,.F.);
#3599=ORIENTED_EDGE('',*,*,#2629,.T.);
#3600=ORIENTED_EDGE('',*,*,#2629,.F.);
#3601=ORIENTED_EDGE('',*,*,#2630,.F.);
#3602=ORIENTED_EDGE('',*,*,#2631,.F.);
#3603=ORIENTED_EDGE('',*,*,#2631,.T.);
#3604=ORIENTED_EDGE('',*,*,#2619,.T.);
#3605=ORIENTED_EDGE('',*,*,#2625,.T.);
#3606=ORIENTED_EDGE('',*,*,#2622,.T.);
#3607=ORIENTED_EDGE('',*,*,#2609,.T.);
#3608=ORIENTED_EDGE('',*,*,#2613,.T.);
#3609=ORIENTED_EDGE('',*,*,#2616,.T.);
#3610=ORIENTED_EDGE('',*,*,#2632,.F.);
#3611=ORIENTED_EDGE('',*,*,#2590,.F.);
#3612=ORIENTED_EDGE('',*,*,#2556,.F.);
#3613=ORIENTED_EDGE('',*,*,#2591,.F.);
#3614=ORIENTED_EDGE('',*,*,#2633,.T.);
#3615=ORIENTED_EDGE('',*,*,#2632,.T.);
#3616=ORIENTED_EDGE('',*,*,#2633,.F.);
#3617=ORIENTED_EDGE('',*,*,#2567,.T.);
#3618=ORIENTED_EDGE('',*,*,#2587,.T.);
#3619=ORIENTED_EDGE('',*,*,#2634,.F.);
#3620=ORIENTED_EDGE('',*,*,#2596,.T.);
#3621=ORIENTED_EDGE('',*,*,#2598,.T.);
#3622=ORIENTED_EDGE('',*,*,#2635,.F.);
#3623=ORIENTED_EDGE('',*,*,#2602,.T.);
#3624=ORIENTED_EDGE('',*,*,#2608,.F.);
#3625=ORIENTED_EDGE('',*,*,#2634,.T.);
#3626=ORIENTED_EDGE('',*,*,#2586,.T.);
#3627=ORIENTED_EDGE('',*,*,#2572,.T.);
#3628=ORIENTED_EDGE('',*,*,#2595,.T.);
#3629=ORIENTED_EDGE('',*,*,#2597,.T.);
#3630=ORIENTED_EDGE('',*,*,#2606,.F.);
#3631=ORIENTED_EDGE('',*,*,#2603,.T.);
#3632=ORIENTED_EDGE('',*,*,#2635,.T.);
#3633=ORIENTED_EDGE('',*,*,#2627,.T.);
#3634=ORIENTED_EDGE('',*,*,#2630,.T.);
#3635=ORIENTED_EDGE('',*,*,#2628,.T.);
#3636=ORIENTED_EDGE('',*,*,#2636,.T.);
#3637=ORIENTED_EDGE('',*,*,#2607,.T.);
#3638=ORIENTED_EDGE('',*,*,#2636,.F.);
#3639=ORIENTED_EDGE('',*,*,#2637,.T.);
#3640=ORIENTED_EDGE('',*,*,#2638,.T.);
#3641=ORIENTED_EDGE('',*,*,#2639,.T.);
#3642=ORIENTED_EDGE('',*,*,#2640,.T.);
#3643=ORIENTED_EDGE('',*,*,#2638,.F.);
#3644=ORIENTED_EDGE('',*,*,#2639,.F.);
#3645=ORIENTED_EDGE('',*,*,#2640,.F.);
#3646=ORIENTED_EDGE('',*,*,#2641,.T.);
#3647=ORIENTED_EDGE('',*,*,#2642,.T.);
#3648=ORIENTED_EDGE('',*,*,#2641,.F.);
#3649=ORIENTED_EDGE('',*,*,#2637,.F.);
#3650=ORIENTED_EDGE('',*,*,#2643,.T.);
#3651=ORIENTED_EDGE('',*,*,#2644,.T.);
#3652=ORIENTED_EDGE('',*,*,#2645,.T.);
#3653=ORIENTED_EDGE('',*,*,#2646,.T.);
#3654=ORIENTED_EDGE('',*,*,#2645,.F.);
#3655=ORIENTED_EDGE('',*,*,#2646,.F.);
#3656=ORIENTED_EDGE('',*,*,#2647,.F.);
#3657=ORIENTED_EDGE('',*,*,#2648,.T.);
#3658=ORIENTED_EDGE('',*,*,#2643,.F.);
#3659=ORIENTED_EDGE('',*,*,#2644,.F.);
#3660=ORIENTED_EDGE('',*,*,#2648,.F.);
#3661=ORIENTED_EDGE('',*,*,#2649,.F.);
#3662=ORIENTED_EDGE('',*,*,#2650,.F.);
#3663=ORIENTED_EDGE('',*,*,#2651,.T.);
#3664=ORIENTED_EDGE('',*,*,#2652,.F.);
#3665=ORIENTED_EDGE('',*,*,#2653,.F.);
#3666=ORIENTED_EDGE('',*,*,#2651,.F.);
#3667=ORIENTED_EDGE('',*,*,#2642,.F.);
#3668=ORIENTED_EDGE('',*,*,#2654,.T.);
#3669=ORIENTED_EDGE('',*,*,#2647,.T.);
#3670=ORIENTED_EDGE('',*,*,#2654,.F.);
#3671=ORIENTED_EDGE('',*,*,#2652,.T.);
#3672=ORIENTED_EDGE('',*,*,#2653,.T.);
#3673=ORIENTED_EDGE('',*,*,#2649,.T.);
#3674=ORIENTED_EDGE('',*,*,#2650,.T.);
#3675=ORIENTED_EDGE('',*,*,#2655,.T.);
#3676=ORIENTED_EDGE('',*,*,#2656,.T.);
#3677=ORIENTED_EDGE('',*,*,#2657,.T.);
#3678=ORIENTED_EDGE('',*,*,#2658,.T.);
#3679=ORIENTED_EDGE('',*,*,#2655,.F.);
#3680=ORIENTED_EDGE('',*,*,#2659,.T.);
#3681=ORIENTED_EDGE('',*,*,#2660,.T.);
#3682=ORIENTED_EDGE('',*,*,#2661,.T.);
#3683=ORIENTED_EDGE('',*,*,#2660,.F.);
#3684=ORIENTED_EDGE('',*,*,#2662,.T.);
#3685=ORIENTED_EDGE('',*,*,#2663,.T.);
#3686=ORIENTED_EDGE('',*,*,#2664,.T.);
#3687=ORIENTED_EDGE('',*,*,#2663,.F.);
#3688=ORIENTED_EDGE('',*,*,#2665,.T.);
#3689=ORIENTED_EDGE('',*,*,#2666,.T.);
#3690=ORIENTED_EDGE('',*,*,#2667,.T.);
#3691=ORIENTED_EDGE('',*,*,#2666,.F.);
#3692=ORIENTED_EDGE('',*,*,#2668,.T.);
#3693=ORIENTED_EDGE('',*,*,#2669,.T.);
#3694=ORIENTED_EDGE('',*,*,#2670,.T.);
#3695=ORIENTED_EDGE('',*,*,#2669,.F.);
#3696=ORIENTED_EDGE('',*,*,#2671,.T.);
#3697=ORIENTED_EDGE('',*,*,#2672,.T.);
#3698=ORIENTED_EDGE('',*,*,#2673,.T.);
#3699=ORIENTED_EDGE('',*,*,#2674,.T.);
#3700=ORIENTED_EDGE('',*,*,#2675,.T.);
#3701=ORIENTED_EDGE('',*,*,#2672,.F.);
#3702=ORIENTED_EDGE('',*,*,#2676,.T.);
#3703=ORIENTED_EDGE('',*,*,#2674,.F.);
#3704=ORIENTED_EDGE('',*,*,#2677,.T.);
#3705=ORIENTED_EDGE('',*,*,#2678,.T.);
#3706=ORIENTED_EDGE('',*,*,#2679,.T.);
#3707=ORIENTED_EDGE('',*,*,#2680,.T.);
#3708=ORIENTED_EDGE('',*,*,#2681,.T.);
#3709=ORIENTED_EDGE('',*,*,#2678,.F.);
#3710=ORIENTED_EDGE('',*,*,#2682,.T.);
#3711=ORIENTED_EDGE('',*,*,#2680,.F.);
#3712=ORIENTED_EDGE('',*,*,#2683,.T.);
#3713=ORIENTED_EDGE('',*,*,#2684,.T.);
#3714=ORIENTED_EDGE('',*,*,#2685,.T.);
#3715=ORIENTED_EDGE('',*,*,#2686,.T.);
#3716=ORIENTED_EDGE('',*,*,#2687,.T.);
#3717=ORIENTED_EDGE('',*,*,#2684,.F.);
#3718=ORIENTED_EDGE('',*,*,#2688,.T.);
#3719=ORIENTED_EDGE('',*,*,#2686,.F.);
#3720=ORIENTED_EDGE('',*,*,#2689,.T.);
#3721=ORIENTED_EDGE('',*,*,#2690,.T.);
#3722=ORIENTED_EDGE('',*,*,#2691,.T.);
#3723=ORIENTED_EDGE('',*,*,#2692,.T.);
#3724=ORIENTED_EDGE('',*,*,#2693,.T.);
#3725=ORIENTED_EDGE('',*,*,#2690,.F.);
#3726=ORIENTED_EDGE('',*,*,#2694,.T.);
#3727=ORIENTED_EDGE('',*,*,#2695,.T.);
#3728=ORIENTED_EDGE('',*,*,#2696,.T.);
#3729=ORIENTED_EDGE('',*,*,#2692,.F.);
#3730=ORIENTED_EDGE('',*,*,#2697,.T.);
#3731=ORIENTED_EDGE('',*,*,#2698,.T.);
#3732=ORIENTED_EDGE('',*,*,#2699,.T.);
#3733=ORIENTED_EDGE('',*,*,#2695,.F.);
#3734=ORIENTED_EDGE('',*,*,#2700,.T.);
#3735=ORIENTED_EDGE('',*,*,#2698,.F.);
#3736=ORIENTED_EDGE('',*,*,#2701,.T.);
#3737=ORIENTED_EDGE('',*,*,#2702,.T.);
#3738=ORIENTED_EDGE('',*,*,#2703,.T.);
#3739=ORIENTED_EDGE('',*,*,#2702,.F.);
#3740=ORIENTED_EDGE('',*,*,#2704,.T.);
#3741=ORIENTED_EDGE('',*,*,#2705,.T.);
#3742=ORIENTED_EDGE('',*,*,#2706,.T.);
#3743=ORIENTED_EDGE('',*,*,#2705,.F.);
#3744=ORIENTED_EDGE('',*,*,#2707,.T.);
#3745=ORIENTED_EDGE('',*,*,#2708,.T.);
#3746=ORIENTED_EDGE('',*,*,#2709,.T.);
#3747=ORIENTED_EDGE('',*,*,#2708,.F.);
#3748=ORIENTED_EDGE('',*,*,#2710,.T.);
#3749=ORIENTED_EDGE('',*,*,#2711,.T.);
#3750=ORIENTED_EDGE('',*,*,#2712,.T.);
#3751=ORIENTED_EDGE('',*,*,#2711,.F.);
#3752=ORIENTED_EDGE('',*,*,#2713,.T.);
#3753=ORIENTED_EDGE('',*,*,#2657,.F.);
#3754=ORIENTED_EDGE('',*,*,#2714,.T.);
#3755=ORIENTED_EDGE('',*,*,#2668,.F.);
#3756=ORIENTED_EDGE('',*,*,#2665,.F.);
#3757=ORIENTED_EDGE('',*,*,#2662,.F.);
#3758=ORIENTED_EDGE('',*,*,#2715,.F.);
#3759=ORIENTED_EDGE('',*,*,#2716,.T.);
#3760=ORIENTED_EDGE('',*,*,#2683,.F.);
#3761=ORIENTED_EDGE('',*,*,#2717,.T.);
#3762=ORIENTED_EDGE('',*,*,#2707,.F.);
#3763=ORIENTED_EDGE('',*,*,#2718,.T.);
#3764=ORIENTED_EDGE('',*,*,#2682,.F.);
#3765=ORIENTED_EDGE('',*,*,#2719,.F.);
#3766=ORIENTED_EDGE('',*,*,#2710,.F.);
#3767=ORIENTED_EDGE('',*,*,#2717,.F.);
#3768=ORIENTED_EDGE('',*,*,#2671,.F.);
#3769=ORIENTED_EDGE('',*,*,#2715,.T.);
#3770=ORIENTED_EDGE('',*,*,#2659,.F.);
#3771=ORIENTED_EDGE('',*,*,#2720,.T.);
#3772=ORIENTED_EDGE('',*,*,#2677,.F.);
#3773=ORIENTED_EDGE('',*,*,#2721,.T.);
#3774=ORIENTED_EDGE('',*,*,#2713,.F.);
#3775=ORIENTED_EDGE('',*,*,#2719,.T.);
#3776=ORIENTED_EDGE('',*,*,#2676,.F.);
#3777=ORIENTED_EDGE('',*,*,#2720,.F.);
#3778=ORIENTED_EDGE('',*,*,#2658,.F.);
#3779=ORIENTED_EDGE('',*,*,#2721,.F.);
#3780=ORIENTED_EDGE('',*,*,#2699,.F.);
#3781=ORIENTED_EDGE('',*,*,#2703,.F.);
#3782=ORIENTED_EDGE('',*,*,#2706,.F.);
#3783=ORIENTED_EDGE('',*,*,#2709,.F.);
#3784=ORIENTED_EDGE('',*,*,#2712,.F.);
#3785=ORIENTED_EDGE('',*,*,#2714,.F.);
#3786=ORIENTED_EDGE('',*,*,#2656,.F.);
#3787=ORIENTED_EDGE('',*,*,#2661,.F.);
#3788=ORIENTED_EDGE('',*,*,#2664,.F.);
#3789=ORIENTED_EDGE('',*,*,#2722,.F.);
#3790=ORIENTED_EDGE('',*,*,#2723,.T.);
#3791=ORIENTED_EDGE('',*,*,#2696,.F.);
#3792=ORIENTED_EDGE('',*,*,#2722,.T.);
#3793=ORIENTED_EDGE('',*,*,#2667,.F.);
#3794=ORIENTED_EDGE('',*,*,#2724,.F.);
#3795=ORIENTED_EDGE('',*,*,#2688,.F.);
#3796=ORIENTED_EDGE('',*,*,#2718,.F.);
#3797=ORIENTED_EDGE('',*,*,#2704,.F.);
#3798=ORIENTED_EDGE('',*,*,#2725,.F.);
#3799=ORIENTED_EDGE('',*,*,#2689,.F.);
#3800=ORIENTED_EDGE('',*,*,#2725,.T.);
#3801=ORIENTED_EDGE('',*,*,#2701,.F.);
#3802=ORIENTED_EDGE('',*,*,#2726,.T.);
#3803=ORIENTED_EDGE('',*,*,#2723,.F.);
#3804=ORIENTED_EDGE('',*,*,#2727,.T.);
#3805=ORIENTED_EDGE('',*,*,#2728,.F.);
#3806=ORIENTED_EDGE('',*,*,#2727,.F.);
#3807=ORIENTED_EDGE('',*,*,#2716,.F.);
#3808=ORIENTED_EDGE('',*,*,#2729,.T.);
#3809=ORIENTED_EDGE('',*,*,#2730,.F.);
#3810=ORIENTED_EDGE('',*,*,#2729,.F.);
#3811=ORIENTED_EDGE('',*,*,#2693,.F.);
#3812=ORIENTED_EDGE('',*,*,#2724,.T.);
#3813=ORIENTED_EDGE('',*,*,#2670,.F.);
#3814=ORIENTED_EDGE('',*,*,#2673,.F.);
#3815=ORIENTED_EDGE('',*,*,#2675,.F.);
#3816=ORIENTED_EDGE('',*,*,#2679,.F.);
#3817=ORIENTED_EDGE('',*,*,#2681,.F.);
#3818=ORIENTED_EDGE('',*,*,#2685,.F.);
#3819=ORIENTED_EDGE('',*,*,#2687,.F.);
#3820=ORIENTED_EDGE('',*,*,#2691,.F.);
#3821=ORIENTED_EDGE('',*,*,#2728,.T.);
#3822=ORIENTED_EDGE('',*,*,#2694,.F.);
#3823=ORIENTED_EDGE('',*,*,#2726,.F.);
#3824=ORIENTED_EDGE('',*,*,#2700,.F.);
#3825=ORIENTED_EDGE('',*,*,#2697,.F.);
#3826=ORIENTED_EDGE('',*,*,#2730,.T.);
#3827=ORIENTED_EDGE('',*,*,#2731,.T.);
#3828=ORIENTED_EDGE('',*,*,#2732,.T.);
#3829=ORIENTED_EDGE('',*,*,#2733,.F.);
#3830=ORIENTED_EDGE('',*,*,#2732,.F.);
#3831=ORIENTED_EDGE('',*,*,#2734,.F.);
#3832=ORIENTED_EDGE('',*,*,#2733,.T.);
#3833=ORIENTED_EDGE('',*,*,#2735,.F.);
#3834=ORIENTED_EDGE('',*,*,#2736,.T.);
#3835=ORIENTED_EDGE('',*,*,#2734,.T.);
#3836=ORIENTED_EDGE('',*,*,#2736,.F.);
#3837=ORIENTED_EDGE('',*,*,#2737,.F.);
#3838=ORIENTED_EDGE('',*,*,#2735,.T.);
#3839=ORIENTED_EDGE('',*,*,#2738,.F.);
#3840=ORIENTED_EDGE('',*,*,#2739,.T.);
#3841=ORIENTED_EDGE('',*,*,#2737,.T.);
#3842=ORIENTED_EDGE('',*,*,#2739,.F.);
#3843=ORIENTED_EDGE('',*,*,#2738,.T.);
#3844=ORIENTED_EDGE('',*,*,#2731,.F.);
#3845=ORIENTED_EDGE('',*,*,#2740,.F.);
#3846=ORIENTED_EDGE('',*,*,#2741,.T.);
#3847=ORIENTED_EDGE('',*,*,#2742,.T.);
#3848=ORIENTED_EDGE('',*,*,#2743,.T.);
#3849=ORIENTED_EDGE('',*,*,#2744,.F.);
#3850=ORIENTED_EDGE('',*,*,#2745,.T.);
#3851=ORIENTED_EDGE('',*,*,#2740,.T.);
#3852=ORIENTED_EDGE('',*,*,#2746,.T.);
#3853=ORIENTED_EDGE('',*,*,#2747,.F.);
#3854=ORIENTED_EDGE('',*,*,#2748,.T.);
#3855=ORIENTED_EDGE('',*,*,#2744,.T.);
#3856=ORIENTED_EDGE('',*,*,#2749,.T.);
#3857=ORIENTED_EDGE('',*,*,#2750,.F.);
#3858=ORIENTED_EDGE('',*,*,#2751,.T.);
#3859=ORIENTED_EDGE('',*,*,#2747,.T.);
#3860=ORIENTED_EDGE('',*,*,#2752,.T.);
#3861=ORIENTED_EDGE('',*,*,#2753,.F.);
#3862=ORIENTED_EDGE('',*,*,#2754,.T.);
#3863=ORIENTED_EDGE('',*,*,#2750,.T.);
#3864=ORIENTED_EDGE('',*,*,#2755,.T.);
#3865=ORIENTED_EDGE('',*,*,#2756,.F.);
#3866=ORIENTED_EDGE('',*,*,#2757,.T.);
#3867=ORIENTED_EDGE('',*,*,#2753,.T.);
#3868=ORIENTED_EDGE('',*,*,#2758,.T.);
#3869=ORIENTED_EDGE('',*,*,#2759,.F.);
#3870=ORIENTED_EDGE('',*,*,#2760,.T.);
#3871=ORIENTED_EDGE('',*,*,#2756,.T.);
#3872=ORIENTED_EDGE('',*,*,#2761,.T.);
#3873=ORIENTED_EDGE('',*,*,#2762,.F.);
#3874=ORIENTED_EDGE('',*,*,#2763,.T.);
#3875=ORIENTED_EDGE('',*,*,#2759,.T.);
#3876=ORIENTED_EDGE('',*,*,#2764,.T.);
#3877=ORIENTED_EDGE('',*,*,#2765,.F.);
#3878=ORIENTED_EDGE('',*,*,#2766,.T.);
#3879=ORIENTED_EDGE('',*,*,#2762,.T.);
#3880=ORIENTED_EDGE('',*,*,#2767,.T.);
#3881=ORIENTED_EDGE('',*,*,#2768,.F.);
#3882=ORIENTED_EDGE('',*,*,#2769,.T.);
#3883=ORIENTED_EDGE('',*,*,#2765,.T.);
#3884=ORIENTED_EDGE('',*,*,#2770,.T.);
#3885=ORIENTED_EDGE('',*,*,#2771,.F.);
#3886=ORIENTED_EDGE('',*,*,#2772,.T.);
#3887=ORIENTED_EDGE('',*,*,#2768,.T.);
#3888=ORIENTED_EDGE('',*,*,#2773,.T.);
#3889=ORIENTED_EDGE('',*,*,#2774,.F.);
#3890=ORIENTED_EDGE('',*,*,#2775,.T.);
#3891=ORIENTED_EDGE('',*,*,#2771,.T.);
#3892=ORIENTED_EDGE('',*,*,#2776,.T.);
#3893=ORIENTED_EDGE('',*,*,#2777,.F.);
#3894=ORIENTED_EDGE('',*,*,#2778,.T.);
#3895=ORIENTED_EDGE('',*,*,#2779,.F.);
#3896=ORIENTED_EDGE('',*,*,#2780,.F.);
#3897=ORIENTED_EDGE('',*,*,#2781,.F.);
#3898=ORIENTED_EDGE('',*,*,#2782,.T.);
#3899=ORIENTED_EDGE('',*,*,#2777,.T.);
#3900=ORIENTED_EDGE('',*,*,#2783,.F.);
#3901=ORIENTED_EDGE('',*,*,#2784,.F.);
#3902=ORIENTED_EDGE('',*,*,#2785,.T.);
#3903=ORIENTED_EDGE('',*,*,#2781,.T.);
#3904=ORIENTED_EDGE('',*,*,#2786,.F.);
#3905=ORIENTED_EDGE('',*,*,#2787,.F.);
#3906=ORIENTED_EDGE('',*,*,#2788,.T.);
#3907=ORIENTED_EDGE('',*,*,#2784,.T.);
#3908=ORIENTED_EDGE('',*,*,#2789,.F.);
#3909=ORIENTED_EDGE('',*,*,#2790,.F.);
#3910=ORIENTED_EDGE('',*,*,#2791,.T.);
#3911=ORIENTED_EDGE('',*,*,#2787,.T.);
#3912=ORIENTED_EDGE('',*,*,#2792,.F.);
#3913=ORIENTED_EDGE('',*,*,#2793,.F.);
#3914=ORIENTED_EDGE('',*,*,#2794,.T.);
#3915=ORIENTED_EDGE('',*,*,#2790,.T.);
#3916=ORIENTED_EDGE('',*,*,#2795,.F.);
#3917=ORIENTED_EDGE('',*,*,#2796,.F.);
#3918=ORIENTED_EDGE('',*,*,#2797,.T.);
#3919=ORIENTED_EDGE('',*,*,#2793,.T.);
#3920=ORIENTED_EDGE('',*,*,#2798,.F.);
#3921=ORIENTED_EDGE('',*,*,#2799,.F.);
#3922=ORIENTED_EDGE('',*,*,#2800,.T.);
#3923=ORIENTED_EDGE('',*,*,#2796,.T.);
#3924=ORIENTED_EDGE('',*,*,#2801,.F.);
#3925=ORIENTED_EDGE('',*,*,#2802,.F.);
#3926=ORIENTED_EDGE('',*,*,#2803,.T.);
#3927=ORIENTED_EDGE('',*,*,#2799,.T.);
#3928=ORIENTED_EDGE('',*,*,#2804,.F.);
#3929=ORIENTED_EDGE('',*,*,#2805,.F.);
#3930=ORIENTED_EDGE('',*,*,#2806,.T.);
#3931=ORIENTED_EDGE('',*,*,#2802,.T.);
#3932=ORIENTED_EDGE('',*,*,#2807,.F.);
#3933=ORIENTED_EDGE('',*,*,#2808,.F.);
#3934=ORIENTED_EDGE('',*,*,#2809,.T.);
#3935=ORIENTED_EDGE('',*,*,#2805,.T.);
#3936=ORIENTED_EDGE('',*,*,#2810,.F.);
#3937=ORIENTED_EDGE('',*,*,#2811,.F.);
#3938=ORIENTED_EDGE('',*,*,#2812,.T.);
#3939=ORIENTED_EDGE('',*,*,#2808,.T.);
#3940=ORIENTED_EDGE('',*,*,#2813,.F.);
#3941=ORIENTED_EDGE('',*,*,#2814,.F.);
#3942=ORIENTED_EDGE('',*,*,#2815,.F.);
#3943=ORIENTED_EDGE('',*,*,#2776,.F.);
#3944=ORIENTED_EDGE('',*,*,#2773,.F.);
#3945=ORIENTED_EDGE('',*,*,#2770,.F.);
#3946=ORIENTED_EDGE('',*,*,#2767,.F.);
#3947=ORIENTED_EDGE('',*,*,#2764,.F.);
#3948=ORIENTED_EDGE('',*,*,#2761,.F.);
#3949=ORIENTED_EDGE('',*,*,#2758,.F.);
#3950=ORIENTED_EDGE('',*,*,#2755,.F.);
#3951=ORIENTED_EDGE('',*,*,#2752,.F.);
#3952=ORIENTED_EDGE('',*,*,#2749,.F.);
#3953=ORIENTED_EDGE('',*,*,#2746,.F.);
#3954=ORIENTED_EDGE('',*,*,#2743,.F.);
#3955=ORIENTED_EDGE('',*,*,#2816,.F.);
#3956=ORIENTED_EDGE('',*,*,#2817,.T.);
#3957=ORIENTED_EDGE('',*,*,#2813,.T.);
#3958=ORIENTED_EDGE('',*,*,#2810,.T.);
#3959=ORIENTED_EDGE('',*,*,#2807,.T.);
#3960=ORIENTED_EDGE('',*,*,#2804,.T.);
#3961=ORIENTED_EDGE('',*,*,#2801,.T.);
#3962=ORIENTED_EDGE('',*,*,#2798,.T.);
#3963=ORIENTED_EDGE('',*,*,#2795,.T.);
#3964=ORIENTED_EDGE('',*,*,#2792,.T.);
#3965=ORIENTED_EDGE('',*,*,#2789,.T.);
#3966=ORIENTED_EDGE('',*,*,#2786,.T.);
#3967=ORIENTED_EDGE('',*,*,#2783,.T.);
#3968=ORIENTED_EDGE('',*,*,#2780,.T.);
#3969=ORIENTED_EDGE('',*,*,#2818,.T.);
#3970=ORIENTED_EDGE('',*,*,#2819,.T.);
#3971=ORIENTED_EDGE('',*,*,#2820,.T.);
#3972=ORIENTED_EDGE('',*,*,#2821,.T.);
#3973=ORIENTED_EDGE('',*,*,#2816,.T.);
#3974=ORIENTED_EDGE('',*,*,#2811,.T.);
#3975=ORIENTED_EDGE('',*,*,#2817,.F.);
#3976=ORIENTED_EDGE('',*,*,#2821,.F.);
#3977=ORIENTED_EDGE('',*,*,#2822,.T.);
#3978=ORIENTED_EDGE('',*,*,#2823,.F.);
#3979=ORIENTED_EDGE('',*,*,#2778,.F.);
#3980=ORIENTED_EDGE('',*,*,#2782,.F.);
#3981=ORIENTED_EDGE('',*,*,#2785,.F.);
#3982=ORIENTED_EDGE('',*,*,#2788,.F.);
#3983=ORIENTED_EDGE('',*,*,#2791,.F.);
#3984=ORIENTED_EDGE('',*,*,#2794,.F.);
#3985=ORIENTED_EDGE('',*,*,#2797,.F.);
#3986=ORIENTED_EDGE('',*,*,#2800,.F.);
#3987=ORIENTED_EDGE('',*,*,#2803,.F.);
#3988=ORIENTED_EDGE('',*,*,#2806,.F.);
#3989=ORIENTED_EDGE('',*,*,#2809,.F.);
#3990=ORIENTED_EDGE('',*,*,#2812,.F.);
#3991=ORIENTED_EDGE('',*,*,#2822,.F.);
#3992=ORIENTED_EDGE('',*,*,#2820,.F.);
#3993=ORIENTED_EDGE('',*,*,#2741,.F.);
#3994=ORIENTED_EDGE('',*,*,#2745,.F.);
#3995=ORIENTED_EDGE('',*,*,#2748,.F.);
#3996=ORIENTED_EDGE('',*,*,#2751,.F.);
#3997=ORIENTED_EDGE('',*,*,#2754,.F.);
#3998=ORIENTED_EDGE('',*,*,#2757,.F.);
#3999=ORIENTED_EDGE('',*,*,#2760,.F.);
#4000=ORIENTED_EDGE('',*,*,#2763,.F.);
#4001=ORIENTED_EDGE('',*,*,#2766,.F.);
#4002=ORIENTED_EDGE('',*,*,#2769,.F.);
#4003=ORIENTED_EDGE('',*,*,#2772,.F.);
#4004=ORIENTED_EDGE('',*,*,#2775,.F.);
#4005=ORIENTED_EDGE('',*,*,#2824,.F.);
#4006=ORIENTED_EDGE('',*,*,#2825,.F.);
#4007=ORIENTED_EDGE('',*,*,#2826,.F.);
#4008=ORIENTED_EDGE('',*,*,#2827,.T.);
#4009=ORIENTED_EDGE('',*,*,#2828,.T.);
#4010=ORIENTED_EDGE('',*,*,#2829,.F.);
#4011=ORIENTED_EDGE('',*,*,#2830,.T.);
#4012=ORIENTED_EDGE('',*,*,#2831,.F.);
#4013=ORIENTED_EDGE('',*,*,#2832,.F.);
#4014=ORIENTED_EDGE('',*,*,#2833,.F.);
#4015=ORIENTED_EDGE('',*,*,#2834,.F.);
#4016=ORIENTED_EDGE('',*,*,#2835,.T.);
#4017=ORIENTED_EDGE('',*,*,#2836,.T.);
#4018=ORIENTED_EDGE('',*,*,#2837,.F.);
#4019=ORIENTED_EDGE('',*,*,#2838,.T.);
#4020=ORIENTED_EDGE('',*,*,#2839,.T.);
#4021=ORIENTED_EDGE('',*,*,#2835,.F.);
#4022=ORIENTED_EDGE('',*,*,#2840,.F.);
#4023=ORIENTED_EDGE('',*,*,#2841,.T.);
#4024=ORIENTED_EDGE('',*,*,#2838,.F.);
#4025=ORIENTED_EDGE('',*,*,#2842,.F.);
#4026=ORIENTED_EDGE('',*,*,#2843,.F.);
#4027=ORIENTED_EDGE('',*,*,#2831,.T.);
#4028=ORIENTED_EDGE('',*,*,#2844,.T.);
#4029=ORIENTED_EDGE('',*,*,#2827,.F.);
#4030=ORIENTED_EDGE('',*,*,#2833,.T.);
#4031=ORIENTED_EDGE('',*,*,#2845,.T.);
#4032=ORIENTED_EDGE('',*,*,#2846,.F.);
#4033=ORIENTED_EDGE('',*,*,#2847,.F.);
#4034=ORIENTED_EDGE('',*,*,#2848,.T.);
#4035=ORIENTED_EDGE('',*,*,#2842,.T.);
#4036=ORIENTED_EDGE('',*,*,#2837,.T.);
#4037=ORIENTED_EDGE('',*,*,#2834,.T.);
#4038=ORIENTED_EDGE('',*,*,#2847,.T.);
#4039=ORIENTED_EDGE('',*,*,#2849,.T.);
#4040=ORIENTED_EDGE('',*,*,#2850,.T.);
#4041=ORIENTED_EDGE('',*,*,#2832,.T.);
#4042=ORIENTED_EDGE('',*,*,#2843,.T.);
#4043=ORIENTED_EDGE('',*,*,#2826,.T.);
#4044=ORIENTED_EDGE('',*,*,#2851,.T.);
#4045=ORIENTED_EDGE('',*,*,#2852,.T.);
#4046=ORIENTED_EDGE('',*,*,#2853,.T.);
#4047=ORIENTED_EDGE('',*,*,#2829,.T.);
#4048=ORIENTED_EDGE('',*,*,#2850,.F.);
#4049=ORIENTED_EDGE('',*,*,#2854,.T.);
#4050=ORIENTED_EDGE('',*,*,#2855,.T.);
#4051=ORIENTED_EDGE('',*,*,#2849,.F.);
#4052=ORIENTED_EDGE('',*,*,#2846,.T.);
#4053=ORIENTED_EDGE('',*,*,#2856,.T.);
#4054=ORIENTED_EDGE('',*,*,#2854,.F.);
#4055=ORIENTED_EDGE('',*,*,#2840,.T.);
#4056=ORIENTED_EDGE('',*,*,#2853,.F.);
#4057=ORIENTED_EDGE('',*,*,#2857,.T.);
#4058=ORIENTED_EDGE('',*,*,#2858,.T.);
#4059=ORIENTED_EDGE('',*,*,#2852,.F.);
#4060=ORIENTED_EDGE('',*,*,#2859,.T.);
#4061=ORIENTED_EDGE('',*,*,#2860,.T.);
#4062=ORIENTED_EDGE('',*,*,#2857,.F.);
#4063=ORIENTED_EDGE('',*,*,#2825,.T.);
#4064=ORIENTED_EDGE('',*,*,#2861,.T.);
#4065=ORIENTED_EDGE('',*,*,#2859,.F.);
#4066=ORIENTED_EDGE('',*,*,#2851,.F.);
#4067=ORIENTED_EDGE('',*,*,#2858,.F.);
#4068=ORIENTED_EDGE('',*,*,#2860,.F.);
#4069=ORIENTED_EDGE('',*,*,#2861,.F.);
#4070=ORIENTED_EDGE('',*,*,#2828,.F.);
#4071=ORIENTED_EDGE('',*,*,#2844,.F.);
#4072=ORIENTED_EDGE('',*,*,#2830,.F.);
#4073=ORIENTED_EDGE('',*,*,#2855,.F.);
#4074=ORIENTED_EDGE('',*,*,#2856,.F.);
#4075=ORIENTED_EDGE('',*,*,#2845,.F.);
#4076=ORIENTED_EDGE('',*,*,#2836,.F.);
#4077=ORIENTED_EDGE('',*,*,#2839,.F.);
#4078=ORIENTED_EDGE('',*,*,#2841,.F.);
#4079=ORIENTED_EDGE('',*,*,#2862,.F.);
#4080=ORIENTED_EDGE('',*,*,#2818,.F.);
#4081=ORIENTED_EDGE('',*,*,#2742,.F.);
#4082=ORIENTED_EDGE('',*,*,#2819,.F.);
#4083=ORIENTED_EDGE('',*,*,#2863,.T.);
#4084=ORIENTED_EDGE('',*,*,#2862,.T.);
#4085=ORIENTED_EDGE('',*,*,#2863,.F.);
#4086=ORIENTED_EDGE('',*,*,#2774,.T.);
#4087=ORIENTED_EDGE('',*,*,#2815,.T.);
#4088=ORIENTED_EDGE('',*,*,#2864,.F.);
#4089=ORIENTED_EDGE('',*,*,#2824,.T.);
#4090=ORIENTED_EDGE('',*,*,#2865,.F.);
#4091=ORIENTED_EDGE('',*,*,#2864,.T.);
#4092=ORIENTED_EDGE('',*,*,#2814,.T.);
#4093=ORIENTED_EDGE('',*,*,#2779,.T.);
#4094=ORIENTED_EDGE('',*,*,#2823,.T.);
#4095=ORIENTED_EDGE('',*,*,#2866,.F.);
#4096=ORIENTED_EDGE('',*,*,#2867,.T.);
#4097=ORIENTED_EDGE('',*,*,#2865,.T.);
#4098=ORIENTED_EDGE('',*,*,#2867,.F.);
#4099=ORIENTED_EDGE('',*,*,#2848,.F.);
#4100=ORIENTED_EDGE('',*,*,#2868,.T.);
#4101=ORIENTED_EDGE('',*,*,#2866,.T.);
#4102=ORIENTED_EDGE('',*,*,#2868,.F.);
#4103=ORIENTED_EDGE('',*,*,#2869,.T.);
#4104=ORIENTED_EDGE('',*,*,#2870,.T.);
#4105=ORIENTED_EDGE('',*,*,#2871,.T.);
#4106=ORIENTED_EDGE('',*,*,#2872,.T.);
#4107=ORIENTED_EDGE('',*,*,#2870,.F.);
#4108=ORIENTED_EDGE('',*,*,#2873,.F.);
#4109=ORIENTED_EDGE('',*,*,#2874,.F.);
#4110=ORIENTED_EDGE('',*,*,#2875,.T.);
#4111=ORIENTED_EDGE('',*,*,#2871,.F.);
#4112=ORIENTED_EDGE('',*,*,#2872,.F.);
#4113=ORIENTED_EDGE('',*,*,#2875,.F.);
#4114=ORIENTED_EDGE('',*,*,#2876,.F.);
#4115=ORIENTED_EDGE('',*,*,#2869,.F.);
#4116=ORIENTED_EDGE('',*,*,#2873,.T.);
#4117=ORIENTED_EDGE('',*,*,#2874,.T.);
#4118=ORIENTED_EDGE('',*,*,#2877,.T.);
#4119=ORIENTED_EDGE('',*,*,#2878,.T.);
#4120=ORIENTED_EDGE('',*,*,#2877,.F.);
#4121=ORIENTED_EDGE('',*,*,#2879,.T.);
#4122=ORIENTED_EDGE('',*,*,#2878,.F.);
#4123=ORIENTED_EDGE('',*,*,#2880,.F.);
#4124=ORIENTED_EDGE('',*,*,#2881,.T.);
#4125=ORIENTED_EDGE('',*,*,#2876,.T.);
#4126=ORIENTED_EDGE('',*,*,#2881,.F.);
#4127=ORIENTED_EDGE('',*,*,#2882,.F.);
#4128=ORIENTED_EDGE('',*,*,#2883,.T.);
#4129=ORIENTED_EDGE('',*,*,#2880,.T.);
#4130=ORIENTED_EDGE('',*,*,#2883,.F.);
#4131=ORIENTED_EDGE('',*,*,#2879,.F.);
#4132=ORIENTED_EDGE('',*,*,#2884,.T.);
#4133=ORIENTED_EDGE('',*,*,#2882,.T.);
#4134=ORIENTED_EDGE('',*,*,#2884,.F.);
#4135=CONICAL_SURFACE('',#4608,2.82,0.785398163397448);
#4136=CONICAL_SURFACE('',#4616,5.105,0.785398163397448);
#4137=CONICAL_SURFACE('',#4626,5.105,0.785398163397448);
#4138=CONICAL_SURFACE('',#4637,3.8,0.785398163397449);
#4139=CONICAL_SURFACE('',#4640,3.8,0.785398163397449);
#4140=CONICAL_SURFACE('',#4643,3.8,0.785398163397449);
#4141=CONICAL_SURFACE('',#4646,3.8,0.785398163397449);
#4142=CONICAL_SURFACE('',#4655,3.8,0.785398163397448);
#4143=CONICAL_SURFACE('',#4658,3.8,0.785398163397448);
#4144=CONICAL_SURFACE('',#4661,3.8,0.785398163397448);
#4145=CONICAL_SURFACE('',#4663,3.8,0.785398163397448);
#4146=CONICAL_SURFACE('',#4678,2.6575,0.683391245487337);
#4147=CONICAL_SURFACE('',#4681,2.6575,0.683391245487336);
#4148=CONICAL_SURFACE('',#4687,3.85,0.982793723247329);
#4149=CONICAL_SURFACE('',#4691,3.9,0.785398163397449);
#4150=CONICAL_SURFACE('',#4697,2.9,0.588002603547568);
#4151=CONICAL_SURFACE('',#4701,3.825,0.244978663126864);
#4152=CONICAL_SURFACE('',#4706,4.275,0.244978663126864);
#4153=CONICAL_SURFACE('',#4710,4.925,0.785398163397449);
#4154=CONICAL_SURFACE('',#4714,4.925,0.78539816339745);
#4155=CONICAL_SURFACE('',#4718,4.275,0.244978663126864);
#4156=CONICAL_SURFACE('',#4722,3.825,0.244978663126864);
#4157=CONICAL_SURFACE('',#4726,3.075,0.78539816339745);
#4158=CONICAL_SURFACE('',#4730,3.075,0.785398163397449);
#4159=CONICAL_SURFACE('',#4752,5.4,0.785398163397448);
#4160=CONICAL_SURFACE('',#4755,2.9,0.785398163397448);
#4161=CONICAL_SURFACE('',#4760,5.4,0.785398163397448);
#4162=CONICAL_SURFACE('',#4765,2.9,0.785398163397448);
#4163=CONICAL_SURFACE('',#4780,2.85,0.785398163397448);
#4164=CONICAL_SURFACE('',#4782,5.35,0.785398163397448);
#4165=CONICAL_SURFACE('',#4790,2.85,0.785398163397448);
#4166=CONICAL_SURFACE('',#4792,5.35,0.785398163397448);
#4167=CONICAL_SURFACE('',#4794,3.16,0.785398163397447);
#4168=CONICAL_SURFACE('',#4837,0.9,0.785398163397448);
#4169=CONICAL_SURFACE('',#4840,0.875,0.896055384571344);
#4170=CONICAL_SURFACE('',#4890,1.15,0.785398163397449);
#4171=CONICAL_SURFACE('',#4898,2.07071067811866,1.17809724509617);
#4172=CONICAL_SURFACE('',#4902,2.3,0.785398163397453);
#4173=CONICAL_SURFACE('',#4905,2.07071067811866,1.17809724509617);
#4174=CONICAL_SURFACE('',#4910,2.3,0.785398163397448);
#4175=CONICAL_SURFACE('',#4916,0.68,0.785398163397448);
#4176=CONICAL_SURFACE('',#4920,2.88,0.785398163397448);
#4177=CONICAL_SURFACE('',#4924,0.68,0.785398163397447);
#4178=CONICAL_SURFACE('',#4928,0.92,0.785398163397448);
#4179=CONICAL_SURFACE('',#4931,3.68,0.785398163397451);
#4180=CONICAL_SURFACE('',#4934,0.92,0.785398163397448);
#4181=CONICAL_SURFACE('',#4938,0.92,0.785398163397445);
#4182=CONICAL_SURFACE('',#4942,2.88,0.785398163397448);
#4183=CONICAL_SURFACE('',#4946,0.92,0.785398163397446);
#4184=CONICAL_SURFACE('',#4950,0.92,0.785398163397448);
#4185=CONICAL_SURFACE('',#4953,3.68,0.785398163397448);
#4186=CONICAL_SURFACE('',#4956,0.92,0.785398163397448);
#4187=CONICAL_SURFACE('',#5039,0.9,0.785398163397448);
#4188=CONICAL_SURFACE('',#5046,1.8,0.674740942223553);
#4189=CONICAL_SURFACE('',#5048,1.35,0.785398163397448);
#4190=CONICAL_SURFACE('',#5057,1.35,0.785398163397448);
#4191=CONICAL_SURFACE('',#5061,1.9,0.785398163397449);
#4192=CONICAL_SURFACE('',#5065,1.9,0.785398163397448);
#4193=ADVANCED_FACE('',(#526),#4135,.T.);
#4194=ADVANCED_FACE('',(#527),#431,.T.);
#4195=ADVANCED_FACE('',(#528,#284),#323,.F.);
#4196=ADVANCED_FACE('',(#529),#4136,.F.);
#4197=ADVANCED_FACE('',(#530,#285),#324,.T.);
#4198=ADVANCED_FACE('',(#531),#432,.F.);
#4199=ADVANCED_FACE('',(#532),#4137,.F.);
#4200=ADVANCED_FACE('',(#533,#286),#325,.F.);
#4201=ADVANCED_FACE('',(#534),#433,.F.);
#4202=ADVANCED_FACE('',(#535),#326,.T.);
#4203=ADVANCED_FACE('',(#536),#4138,.T.);
#4204=ADVANCED_FACE('',(#537),#327,.T.);
#4205=ADVANCED_FACE('',(#538),#4139,.T.);
#4206=ADVANCED_FACE('',(#539),#328,.T.);
#4207=ADVANCED_FACE('',(#540),#4140,.T.);
#4208=ADVANCED_FACE('',(#541),#329,.T.);
#4209=ADVANCED_FACE('',(#542),#4141,.T.);
#4210=ADVANCED_FACE('',(#543),#434,.T.);
#4211=ADVANCED_FACE('',(#544),#330,.T.);
#4212=ADVANCED_FACE('',(#545),#435,.T.);
#4213=ADVANCED_FACE('',(#546),#331,.T.);
#4214=ADVANCED_FACE('',(#547),#332,.T.);
#4215=ADVANCED_FACE('',(#548),#4142,.T.);
#4216=ADVANCED_FACE('',(#549),#333,.T.);
#4217=ADVANCED_FACE('',(#550),#4143,.T.);
#4218=ADVANCED_FACE('',(#551),#334,.T.);
#4219=ADVANCED_FACE('',(#552),#4144,.T.);
#4220=ADVANCED_FACE('',(#553),#335,.T.);
#4221=ADVANCED_FACE('',(#554),#4145,.T.);
#4222=ADVANCED_FACE('',(#555),#436,.T.);
#4223=ADVANCED_FACE('',(#556),#336,.T.);
#4224=ADVANCED_FACE('',(#557),#437,.T.);
#4225=ADVANCED_FACE('',(#558),#337,.T.);
#4226=ADVANCED_FACE('',(#559),#438,.F.);
#4227=ADVANCED_FACE('',(#560),#338,.F.);
#4228=ADVANCED_FACE('',(#561,#287),#339,.F.);
#4229=ADVANCED_FACE('',(#562),#439,.F.);
#4230=ADVANCED_FACE('',(#563,#288),#340,.F.);
#4231=ADVANCED_FACE('',(#564),#341,.T.);
#4232=ADVANCED_FACE('',(#565),#4146,.F.);
#4233=ADVANCED_FACE('',(#566),#4147,.F.);
#4234=ADVANCED_FACE('',(#567),#440,.F.);
#4235=ADVANCED_FACE('',(#568,#289),#342,.T.);
#4236=ADVANCED_FACE('',(#569),#4148,.T.);
#4237=ADVANCED_FACE('',(#570),#441,.T.);
#4238=ADVANCED_FACE('',(#571),#4149,.T.);
#4239=ADVANCED_FACE('',(#572,#290),#343,.T.);
#4240=ADVANCED_FACE('',(#573),#442,.T.);
#4241=ADVANCED_FACE('',(#574),#4150,.T.);
#4242=ADVANCED_FACE('',(#575,#291),#344,.T.);
#4243=ADVANCED_FACE('',(#576),#4151,.T.);
#4244=ADVANCED_FACE('',(#577,#292),#345,.T.);
#4245=ADVANCED_FACE('',(#578),#4152,.F.);
#4246=ADVANCED_FACE('',(#579,#293),#346,.T.);
#4247=ADVANCED_FACE('',(#580),#4153,.T.);
#4248=ADVANCED_FACE('',(#581),#443,.T.);
#4249=ADVANCED_FACE('',(#582),#4154,.T.);
#4250=ADVANCED_FACE('',(#583,#294),#347,.T.);
#4251=ADVANCED_FACE('',(#584),#4155,.F.);
#4252=ADVANCED_FACE('',(#585,#295),#348,.T.);
#4253=ADVANCED_FACE('',(#586),#4156,.T.);
#4254=ADVANCED_FACE('',(#587,#296),#349,.T.);
#4255=ADVANCED_FACE('',(#588),#4157,.F.);
#4256=ADVANCED_FACE('',(#589),#444,.F.);
#4257=ADVANCED_FACE('',(#590),#4158,.F.);
#4258=ADVANCED_FACE('',(#591,#297),#350,.T.);
#4259=ADVANCED_FACE('',(#592),#445,.F.);
#4260=ADVANCED_FACE('',(#593,#298),#351,.T.);
#4261=ADVANCED_FACE('',(#594),#446,.T.);
#4262=ADVANCED_FACE('',(#595,#299),#352,.T.);
#4263=ADVANCED_FACE('',(#596),#353,.T.);
#4264=ADVANCED_FACE('',(#597),#354,.T.);
#4265=ADVANCED_FACE('',(#598),#355,.T.);
#4266=ADVANCED_FACE('',(#599),#356,.T.);
#4267=ADVANCED_FACE('',(#600),#357,.T.);
#4268=ADVANCED_FACE('',(#601),#358,.T.);
#4269=ADVANCED_FACE('',(#602),#359,.T.);
#4270=ADVANCED_FACE('',(#603),#360,.T.);
#4271=ADVANCED_FACE('',(#604),#361,.T.);
#4272=ADVANCED_FACE('',(#605),#4159,.T.);
#4273=ADVANCED_FACE('',(#606),#4160,.T.);
#4274=ADVANCED_FACE('',(#607),#362,.T.);
#4275=ADVANCED_FACE('',(#608),#363,.T.);
#4276=ADVANCED_FACE('',(#609),#4161,.T.);
#4277=ADVANCED_FACE('',(#610),#364,.T.);
#4278=ADVANCED_FACE('',(#611),#4162,.T.);
#4279=ADVANCED_FACE('',(#612),#447,.T.);
#4280=ADVANCED_FACE('',(#613),#448,.T.);
#4281=ADVANCED_FACE('',(#614),#449,.T.);
#4282=ADVANCED_FACE('',(#615),#450,.T.);
#4283=ADVANCED_FACE('',(#616,#300,#301,#302),#365,.F.);
#4284=ADVANCED_FACE('',(#617),#4163,.T.);
#4285=ADVANCED_FACE('',(#618),#4164,.T.);
#4286=ADVANCED_FACE('',(#619),#451,.T.);
#4287=ADVANCED_FACE('',(#620),#452,.F.);
#4288=ADVANCED_FACE('',(#621),#4165,.T.);
#4289=ADVANCED_FACE('',(#622),#4166,.T.);
#4290=ADVANCED_FACE('',(#623),#4167,.F.);
#4291=ADVANCED_FACE('',(#624,#303,#304,#305),#366,.T.);
#4292=ADVANCED_FACE('',(#625),#367,.T.);
#4293=ADVANCED_FACE('',(#626),#368,.T.);
#4294=ADVANCED_FACE('',(#627),#453,.F.);
#4295=ADVANCED_FACE('',(#628),#454,.F.);
#4296=ADVANCED_FACE('',(#629),#455,.F.);
#4297=ADVANCED_FACE('',(#630),#456,.T.);
#4298=ADVANCED_FACE('',(#631),#457,.T.);
#4299=ADVANCED_FACE('',(#632),#458,.T.);
#4300=ADVANCED_FACE('',(#633),#459,.T.);
#4301=ADVANCED_FACE('',(#634),#460,.T.);
#4302=ADVANCED_FACE('',(#635),#461,.T.);
#4303=ADVANCED_FACE('',(#636),#462,.T.);
#4304=ADVANCED_FACE('',(#637),#463,.T.);
#4305=ADVANCED_FACE('',(#638),#464,.T.);
#4306=ADVANCED_FACE('',(#639),#465,.T.);
#4307=ADVANCED_FACE('',(#640),#466,.T.);
#4308=ADVANCED_FACE('',(#641),#369,.F.);
#4309=ADVANCED_FACE('',(#642),#80,.F.);
#4310=ADVANCED_FACE('',(#643),#370,.T.);
#4311=ADVANCED_FACE('',(#644),#467,.T.);
#4312=ADVANCED_FACE('',(#645),#81,.F.);
#4313=ADVANCED_FACE('',(#646),#371,.F.);
#4314=ADVANCED_FACE('',(#647),#372,.F.);
#4315=ADVANCED_FACE('',(#648),#373,.F.);
#4316=ADVANCED_FACE('',(#649),#374,.F.);
#4317=ADVANCED_FACE('',(#650),#375,.F.);
#4318=ADVANCED_FACE('',(#651),#376,.F.);
#4319=ADVANCED_FACE('',(#652),#377,.F.);
#4320=ADVANCED_FACE('',(#653,#306),#378,.T.);
#4321=ADVANCED_FACE('',(#654),#4168,.T.);
#4322=ADVANCED_FACE('',(#655),#468,.T.);
#4323=ADVANCED_FACE('',(#656),#4169,.T.);
#4324=ADVANCED_FACE('',(#657),#379,.T.);
#4325=ADVANCED_FACE('',(#658),#469,.T.);
#4326=ADVANCED_FACE('',(#659),#470,.T.);
#4327=ADVANCED_FACE('',(#660),#471,.T.);
#4328=ADVANCED_FACE('',(#661),#472,.T.);
#4329=ADVANCED_FACE('',(#662),#473,.T.);
#4330=ADVANCED_FACE('',(#663),#474,.T.);
#4331=ADVANCED_FACE('',(#664),#475,.T.);
#4332=ADVANCED_FACE('',(#665),#476,.T.);
#4333=ADVANCED_FACE('',(#666),#477,.T.);
#4334=ADVANCED_FACE('',(#667),#478,.T.);
#4335=ADVANCED_FACE('',(#668),#82,.F.);
#4336=ADVANCED_FACE('',(#669),#380,.T.);
#4337=ADVANCED_FACE('',(#670),#479,.T.);
#4338=ADVANCED_FACE('',(#671),#83,.F.);
#4339=ADVANCED_FACE('',(#672),#381,.F.);
#4340=ADVANCED_FACE('',(#673),#382,.F.);
#4341=ADVANCED_FACE('',(#674,#307),#383,.T.);
#4342=ADVANCED_FACE('',(#675),#480,.T.);
#4343=ADVANCED_FACE('',(#676),#384,.F.);
#4344=ADVANCED_FACE('',(#677),#385,.F.);
#4345=ADVANCED_FACE('',(#678),#386,.F.);
#4346=ADVANCED_FACE('',(#679),#387,.F.);
#4347=ADVANCED_FACE('',(#680),#388,.F.);
#4348=ADVANCED_FACE('',(#681),#389,.F.);
#4349=ADVANCED_FACE('',(#682),#390,.F.);
#4350=ADVANCED_FACE('',(#683,#308),#79,.T.);
#4351=ADVANCED_FACE('',(#684),#391,.T.);
#4352=ADVANCED_FACE('',(#685),#4170,.T.);
#4353=ADVANCED_FACE('',(#686),#481,.T.);
#4354=ADVANCED_FACE('',(#687,#309),#392,.T.);
#4355=ADVANCED_FACE('',(#688),#482,.T.);
#4356=ADVANCED_FACE('',(#689),#483,.T.);
#4357=ADVANCED_FACE('',(#690),#4171,.T.);
#4358=ADVANCED_FACE('',(#691),#4172,.T.);
#4359=ADVANCED_FACE('',(#692),#393,.T.);
#4360=ADVANCED_FACE('',(#693),#4173,.T.);
#4361=ADVANCED_FACE('',(#694),#394,.T.);
#4362=ADVANCED_FACE('',(#695),#4174,.T.);
#4363=ADVANCED_FACE('',(#696),#484,.F.);
#4364=ADVANCED_FACE('',(#697,#310,#311),#485,.T.);
#4365=ADVANCED_FACE('',(#698),#395,.T.);
#4366=ADVANCED_FACE('',(#699),#4175,.T.);
#4367=ADVANCED_FACE('',(#700),#396,.T.);
#4368=ADVANCED_FACE('',(#701),#4176,.T.);
#4369=ADVANCED_FACE('',(#702),#397,.T.);
#4370=ADVANCED_FACE('',(#703),#4177,.T.);
#4371=ADVANCED_FACE('',(#704),#398,.T.);
#4372=ADVANCED_FACE('',(#705),#4178,.F.);
#4373=ADVANCED_FACE('',(#706),#4179,.T.);
#4374=ADVANCED_FACE('',(#707),#4180,.F.);
#4375=ADVANCED_FACE('',(#708),#399,.T.);
#4376=ADVANCED_FACE('',(#709),#4181,.F.);
#4377=ADVANCED_FACE('',(#710),#400,.T.);
#4378=ADVANCED_FACE('',(#711),#4182,.T.);
#4379=ADVANCED_FACE('',(#712),#401,.T.);
#4380=ADVANCED_FACE('',(#713),#4183,.F.);
#4381=ADVANCED_FACE('',(#714),#402,.T.);
#4382=ADVANCED_FACE('',(#715),#4184,.F.);
#4383=ADVANCED_FACE('',(#716),#4185,.T.);
#4384=ADVANCED_FACE('',(#717),#4186,.F.);
#4385=ADVANCED_FACE('',(#718,#312),#403,.T.);
#4386=ADVANCED_FACE('',(#719),#486,.F.);
#4387=ADVANCED_FACE('',(#720),#487,.T.);
#4388=ADVANCED_FACE('',(#721),#488,.T.);
#4389=ADVANCED_FACE('',(#722),#489,.F.);
#4390=ADVANCED_FACE('',(#723),#404,.T.);
#4391=ADVANCED_FACE('',(#724,#313),#405,.T.);
#4392=ADVANCED_FACE('',(#725),#490,.T.);
#4393=ADVANCED_FACE('',(#726),#406,.T.);
#4394=ADVANCED_FACE('',(#727),#491,.F.);
#4395=ADVANCED_FACE('',(#728),#492,.F.);
#4396=ADVANCED_FACE('',(#729),#493,.F.);
#4397=ADVANCED_FACE('',(#730,#314),#407,.T.);
#4398=ADVANCED_FACE('',(#731,#315),#408,.F.);
#4399=ADVANCED_FACE('',(#732),#494,.F.);
#4400=ADVANCED_FACE('',(#733,#316),#409,.T.);
#4401=ADVANCED_FACE('',(#734),#495,.T.);
#4402=ADVANCED_FACE('',(#735,#317),#410,.T.);
#4403=ADVANCED_FACE('',(#736),#496,.T.);
#4404=ADVANCED_FACE('',(#737,#318),#411,.T.);
#4405=ADVANCED_FACE('',(#738),#497,.T.);
#4406=ADVANCED_FACE('',(#739),#498,.T.);
#4407=ADVANCED_FACE('',(#740),#499,.T.);
#4408=ADVANCED_FACE('',(#741),#500,.T.);
#4409=ADVANCED_FACE('',(#742),#501,.T.);
#4410=ADVANCED_FACE('',(#743),#502,.T.);
#4411=ADVANCED_FACE('',(#744),#503,.T.);
#4412=ADVANCED_FACE('',(#745),#504,.T.);
#4413=ADVANCED_FACE('',(#746),#505,.T.);
#4414=ADVANCED_FACE('',(#747),#506,.T.);
#4415=ADVANCED_FACE('',(#748),#507,.T.);
#4416=ADVANCED_FACE('',(#749),#508,.T.);
#4417=ADVANCED_FACE('',(#750),#509,.T.);
#4418=ADVANCED_FACE('',(#751),#510,.T.);
#4419=ADVANCED_FACE('',(#752),#511,.T.);
#4420=ADVANCED_FACE('',(#753),#512,.T.);
#4421=ADVANCED_FACE('',(#754),#513,.T.);
#4422=ADVANCED_FACE('',(#755),#514,.T.);
#4423=ADVANCED_FACE('',(#756),#515,.T.);
#4424=ADVANCED_FACE('',(#757),#516,.T.);
#4425=ADVANCED_FACE('',(#758),#517,.T.);
#4426=ADVANCED_FACE('',(#759),#518,.T.);
#4427=ADVANCED_FACE('',(#760),#519,.T.);
#4428=ADVANCED_FACE('',(#761),#520,.T.);
#4429=ADVANCED_FACE('',(#762),#84,.F.);
#4430=ADVANCED_FACE('',(#763),#412,.T.);
#4431=ADVANCED_FACE('',(#764),#521,.T.);
#4432=ADVANCED_FACE('',(#765),#85,.F.);
#4433=ADVANCED_FACE('',(#766),#413,.F.);
#4434=ADVANCED_FACE('',(#767),#414,.F.);
#4435=ADVANCED_FACE('',(#768),#415,.F.);
#4436=ADVANCED_FACE('',(#769),#416,.F.);
#4437=ADVANCED_FACE('',(#770),#417,.F.);
#4438=ADVANCED_FACE('',(#771),#418,.F.);
#4439=ADVANCED_FACE('',(#772),#419,.F.);
#4440=ADVANCED_FACE('',(#773,#319),#420,.T.);
#4441=ADVANCED_FACE('',(#774),#421,.F.);
#4442=ADVANCED_FACE('',(#775),#422,.F.);
#4443=ADVANCED_FACE('',(#776),#423,.F.);
#4444=ADVANCED_FACE('',(#777),#424,.F.);
#4445=ADVANCED_FACE('',(#778),#425,.F.);
#4446=ADVANCED_FACE('',(#779),#426,.F.);
#4447=ADVANCED_FACE('',(#780),#427,.T.);
#4448=ADVANCED_FACE('',(#781),#4187,.T.);
#4449=ADVANCED_FACE('',(#782),#522,.T.);
#4450=ADVANCED_FACE('',(#783,#320),#428,.T.);
#4451=ADVANCED_FACE('',(#784),#523,.T.);
#4452=ADVANCED_FACE('',(#785),#4188,.T.);
#4453=ADVANCED_FACE('',(#786),#4189,.F.);
#4454=ADVANCED_FACE('',(#787),#524,.F.);
#4455=ADVANCED_FACE('',(#788,#321),#429,.T.);
#4456=ADVANCED_FACE('',(#789),#4190,.F.);
#4457=ADVANCED_FACE('',(#790,#322),#430,.T.);
#4458=ADVANCED_FACE('',(#791),#4191,.T.);
#4459=ADVANCED_FACE('',(#792),#525,.T.);
#4460=ADVANCED_FACE('',(#793),#4192,.T.);
#4461=CLOSED_SHELL('',(#4193,#4194,#4195,#4196,#4197,#4198,#4199,#4200,
#4201,#4202,#4203,#4204,#4205,#4206,#4207,#4208,#4209,#4210,#4211,#4212,
#4213,#4214,#4215,#4216,#4217,#4218,#4219,#4220,#4221,#4222,#4223,#4224,
#4225,#4226,#4227,#4228,#4229,#4230,#4231));
#4462=CLOSED_SHELL('',(#4232,#4233,#4234,#4235,#4236,#4237,#4238,#4239,
#4240,#4241,#4242));
#4463=CLOSED_SHELL('',(#4243,#4244,#4245,#4246,#4247,#4248,#4249,#4250,
#4251,#4252,#4253,#4254,#4255,#4256,#4257,#4258));
#4464=CLOSED_SHELL('',(#4259,#4260,#4261,#4262));
#4465=CLOSED_SHELL('',(#4263,#4264,#4265,#4266,#4267,#4268,#4269,#4270,
#4271,#4272,#4273,#4274,#4275,#4276,#4277,#4278,#4279,#4280,#4281,#4282,
#4283,#4284,#4285,#4286,#4287,#4288,#4289,#4290,#4291,#4292,#4293,#4294,
#4295,#4296));
#4466=CLOSED_SHELL('',(#4297,#4298,#4299,#4300,#4301,#4302,#4303,#4304,
#4305,#4306,#4307,#4308,#4309,#4310,#4311,#4312,#4313,#4314,#4315,#4316,
#4317,#4318,#4319,#4320,#4321,#4322,#4323,#4324));
#4467=CLOSED_SHELL('',(#4325,#4326,#4327,#4328,#4329,#4330,#4331,#4332,
#4333,#4334,#4335,#4336,#4337,#4338,#4339,#4340,#4341,#4342,#4343,#4344,
#4345,#4346,#4347,#4348,#4349,#4350,#4351,#4352,#4353,#4354,#4355,#4356));
#4468=CLOSED_SHELL('',(#4357,#4358,#4359,#4360,#4361,#4362,#4363,#4364));
#4469=CLOSED_SHELL('',(#4365,#4366,#4367,#4368,#4369,#4370,#4371,#4372,
#4373,#4374,#4375,#4376,#4377,#4378,#4379,#4380,#4381,#4382,#4383,#4384,
#4385,#4386,#4387,#4388,#4389,#4390,#4391,#4392,#4393,#4394,#4395,#4396,
#4397,#4398));
#4470=CLOSED_SHELL('',(#4399,#4400,#4401,#4402,#4403,#4404));
#4471=CLOSED_SHELL('',(#4405,#4406,#4407,#4408,#4409,#4410,#4411,#4412,
#4413,#4414,#4415,#4416,#4417,#4418,#4419,#4420,#4421,#4422,#4423,#4424,
#4425,#4426,#4427,#4428,#4429,#4430,#4431,#4432,#4433,#4434,#4435,#4436,
#4437,#4438,#4439,#4440,#4441,#4442,#4443,#4444,#4445,#4446,#4447,#4448,
#4449,#4450,#4451,#4452));
#4472=CLOSED_SHELL('',(#4453,#4454,#4455,#4456,#4457,#4458,#4459,#4460));
#4473=DERIVED_UNIT_ELEMENT(#4497,1.);
#4474=DERIVED_UNIT_ELEMENT(#11432,-3.);
#4475=DERIVED_UNIT_ELEMENT(#4497,1.);
#4476=DERIVED_UNIT_ELEMENT(#11432,-3.);
#4477=DERIVED_UNIT_ELEMENT(#4497,1.);
#4478=DERIVED_UNIT_ELEMENT(#11432,-3.);
#4479=DERIVED_UNIT_ELEMENT(#4497,1.);
#4480=DERIVED_UNIT_ELEMENT(#11432,-3.);
#4481=DERIVED_UNIT_ELEMENT(#4497,1.);
#4482=DERIVED_UNIT_ELEMENT(#11432,-3.);
#4483=DERIVED_UNIT_ELEMENT(#4497,1.);
#4484=DERIVED_UNIT_ELEMENT(#11432,-3.);
#4485=DERIVED_UNIT_ELEMENT(#4497,1.);
#4486=DERIVED_UNIT_ELEMENT(#11432,-3.);
#4487=DERIVED_UNIT_ELEMENT(#4497,1.);
#4488=DERIVED_UNIT_ELEMENT(#11432,-3.);
#4489=DERIVED_UNIT_ELEMENT(#4497,1.);
#4490=DERIVED_UNIT_ELEMENT(#11432,-3.);
#4491=DERIVED_UNIT_ELEMENT(#4497,1.);
#4492=DERIVED_UNIT_ELEMENT(#11432,-3.);
#4493=DERIVED_UNIT_ELEMENT(#4497,1.);
#4494=DERIVED_UNIT_ELEMENT(#11432,-3.);
#4495=DERIVED_UNIT_ELEMENT(#4497,1.);
#4496=DERIVED_UNIT_ELEMENT(#11432,-3.);
#4497=(
MASS_UNIT()
NAMED_UNIT(*)
SI_UNIT(.KILO.,.GRAM.)
);
#4498=DERIVED_UNIT((#4473,#4474));
#4499=DERIVED_UNIT((#4475,#4476));
#4500=DERIVED_UNIT((#4477,#4478));
#4501=DERIVED_UNIT((#4479,#4480));
#4502=DERIVED_UNIT((#4481,#4482));
#4503=DERIVED_UNIT((#4483,#4484));
#4504=DERIVED_UNIT((#4485,#4486));
#4505=DERIVED_UNIT((#4487,#4488));
#4506=DERIVED_UNIT((#4489,#4490));
#4507=DERIVED_UNIT((#4491,#4492));
#4508=DERIVED_UNIT((#4493,#4494));
#4509=DERIVED_UNIT((#4495,#4496));
#4510=MEASURE_REPRESENTATION_ITEM('density measure',
POSITIVE_RATIO_MEASURE(7850.),#4498);
#4511=MEASURE_REPRESENTATION_ITEM('density measure',
POSITIVE_RATIO_MEASURE(7850.),#4499);
#4512=MEASURE_REPRESENTATION_ITEM('density measure',
POSITIVE_RATIO_MEASURE(7850.),#4500);
#4513=MEASURE_REPRESENTATION_ITEM('density measure',
POSITIVE_RATIO_MEASURE(7850.),#4501);
#4514=MEASURE_REPRESENTATION_ITEM('density measure',
POSITIVE_RATIO_MEASURE(7850.),#4502);
#4515=MEASURE_REPRESENTATION_ITEM('density measure',
POSITIVE_RATIO_MEASURE(7850.),#4503);
#4516=MEASURE_REPRESENTATION_ITEM('density measure',
POSITIVE_RATIO_MEASURE(7850.),#4504);
#4517=MEASURE_REPRESENTATION_ITEM('density measure',
POSITIVE_RATIO_MEASURE(7850.),#4505);
#4518=MEASURE_REPRESENTATION_ITEM('density measure',
POSITIVE_RATIO_MEASURE(7850.),#4506);
#4519=MEASURE_REPRESENTATION_ITEM('density measure',
POSITIVE_RATIO_MEASURE(7850.),#4507);
#4520=MEASURE_REPRESENTATION_ITEM('density measure',
POSITIVE_RATIO_MEASURE(7850.),#4508);
#4521=MEASURE_REPRESENTATION_ITEM('density measure',
POSITIVE_RATIO_MEASURE(7850.),#4509);
#4522=PROPERTY_DEFINITION_REPRESENTATION(#4582,#4546);
#4523=PROPERTY_DEFINITION_REPRESENTATION(#4583,#4547);
#4524=PROPERTY_DEFINITION_REPRESENTATION(#4584,#4548);
#4525=PROPERTY_DEFINITION_REPRESENTATION(#4585,#4549);
#4526=PROPERTY_DEFINITION_REPRESENTATION(#4586,#4550);
#4527=PROPERTY_DEFINITION_REPRESENTATION(#4587,#4551);
#4528=PROPERTY_DEFINITION_REPRESENTATION(#4588,#4552);
#4529=PROPERTY_DEFINITION_REPRESENTATION(#4589,#4553);
#4530=PROPERTY_DEFINITION_REPRESENTATION(#4590,#4554);
#4531=PROPERTY_DEFINITION_REPRESENTATION(#4591,#4555);
#4532=PROPERTY_DEFINITION_REPRESENTATION(#4592,#4556);
#4533=PROPERTY_DEFINITION_REPRESENTATION(#4593,#4557);
#4534=PROPERTY_DEFINITION_REPRESENTATION(#4594,#4558);
#4535=PROPERTY_DEFINITION_REPRESENTATION(#4595,#4559);
#4536=PROPERTY_DEFINITION_REPRESENTATION(#4596,#4560);
#4537=PROPERTY_DEFINITION_REPRESENTATION(#4597,#4561);
#4538=PROPERTY_DEFINITION_REPRESENTATION(#4598,#4562);
#4539=PROPERTY_DEFINITION_REPRESENTATION(#4599,#4563);
#4540=PROPERTY_DEFINITION_REPRESENTATION(#4600,#4564);
#4541=PROPERTY_DEFINITION_REPRESENTATION(#4601,#4565);
#4542=PROPERTY_DEFINITION_REPRESENTATION(#4602,#4566);
#4543=PROPERTY_DEFINITION_REPRESENTATION(#4603,#4567);
#4544=PROPERTY_DEFINITION_REPRESENTATION(#4604,#4568);
#4545=PROPERTY_DEFINITION_REPRESENTATION(#4605,#4569);
#4546=REPRESENTATION('material name',(#4570),#11418);
#4547=REPRESENTATION('density',(#4510),#11418);
#4548=REPRESENTATION('material name',(#4571),#11419);
#4549=REPRESENTATION('density',(#4511),#11419);
#4550=REPRESENTATION('material name',(#4572),#11420);
#4551=REPRESENTATION('density',(#4512),#11420);
#4552=REPRESENTATION('material name',(#4573),#11421);
#4553=REPRESENTATION('density',(#4513),#11421);
#4554=REPRESENTATION('material name',(#4574),#11422);
#4555=REPRESENTATION('density',(#4514),#11422);
#4556=REPRESENTATION('material name',(#4575),#11423);
#4557=REPRESENTATION('density',(#4515),#11423);
#4558=REPRESENTATION('material name',(#4576),#11424);
#4559=REPRESENTATION('density',(#4516),#11424);
#4560=REPRESENTATION('material name',(#4577),#11425);
#4561=REPRESENTATION('density',(#4517),#11425);
#4562=REPRESENTATION('material name',(#4578),#11426);
#4563=REPRESENTATION('density',(#4518),#11426);
#4564=REPRESENTATION('material name',(#4579),#11427);
#4565=REPRESENTATION('density',(#4519),#11427);
#4566=REPRESENTATION('material name',(#4580),#11428);
#4567=REPRESENTATION('density',(#4520),#11428);
#4568=REPRESENTATION('material name',(#4581),#11429);
#4569=REPRESENTATION('density',(#4521),#11429);
#4570=DESCRIPTIVE_REPRESENTATION_ITEM('Steel','Steel');
#4571=DESCRIPTIVE_REPRESENTATION_ITEM('Steel','Steel');
#4572=DESCRIPTIVE_REPRESENTATION_ITEM('Steel','Steel');
#4573=DESCRIPTIVE_REPRESENTATION_ITEM('Steel','Steel');
#4574=DESCRIPTIVE_REPRESENTATION_ITEM('Steel','Steel');
#4575=DESCRIPTIVE_REPRESENTATION_ITEM('Steel','Steel');
#4576=DESCRIPTIVE_REPRESENTATION_ITEM('Steel','Steel');
#4577=DESCRIPTIVE_REPRESENTATION_ITEM('Steel','Steel');
#4578=DESCRIPTIVE_REPRESENTATION_ITEM('Steel','Steel');
#4579=DESCRIPTIVE_REPRESENTATION_ITEM('Steel','Steel');
#4580=DESCRIPTIVE_REPRESENTATION_ITEM('Steel','Steel');
#4581=DESCRIPTIVE_REPRESENTATION_ITEM('Steel','Steel');
#4582=PROPERTY_DEFINITION('material property','material name',#11493);
#4583=PROPERTY_DEFINITION('material property','density of part',#11493);
#4584=PROPERTY_DEFINITION('material property','material name',#11494);
#4585=PROPERTY_DEFINITION('material property','density of part',#11494);
#4586=PROPERTY_DEFINITION('material property','material name',#11495);
#4587=PROPERTY_DEFINITION('material property','density of part',#11495);
#4588=PROPERTY_DEFINITION('material property','material name',#11496);
#4589=PROPERTY_DEFINITION('material property','density of part',#11496);
#4590=PROPERTY_DEFINITION('material property','material name',#11497);
#4591=PROPERTY_DEFINITION('material property','density of part',#11497);
#4592=PROPERTY_DEFINITION('material property','material name',#11498);
#4593=PROPERTY_DEFINITION('material property','density of part',#11498);
#4594=PROPERTY_DEFINITION('material property','material name',#11499);
#4595=PROPERTY_DEFINITION('material property','density of part',#11499);
#4596=PROPERTY_DEFINITION('material property','material name',#11500);
#4597=PROPERTY_DEFINITION('material property','density of part',#11500);
#4598=PROPERTY_DEFINITION('material property','material name',#11501);
#4599=PROPERTY_DEFINITION('material property','density of part',#11501);
#4600=PROPERTY_DEFINITION('material property','material name',#11502);
#4601=PROPERTY_DEFINITION('material property','density of part',#11502);
#4602=PROPERTY_DEFINITION('material property','material name',#11503);
#4603=PROPERTY_DEFINITION('material property','density of part',#11503);
#4604=PROPERTY_DEFINITION('material property','material name',#11504);
#4605=PROPERTY_DEFINITION('material property','density of part',#11504);
#4606=AXIS2_PLACEMENT_3D('',#6327,#5083,#5084);
#4607=AXIS2_PLACEMENT_3D('',#6328,#5085,#5086);
#4608=AXIS2_PLACEMENT_3D('',#6329,#5087,#5088);
#4609=AXIS2_PLACEMENT_3D('',#6331,#5089,#5090);
#4610=AXIS2_PLACEMENT_3D('',#6334,#5092,#5093);
#4611=AXIS2_PLACEMENT_3D('',#6335,#5094,#5095);
#4612=AXIS2_PLACEMENT_3D('',#6339,#5097,#5098);
#4613=AXIS2_PLACEMENT_3D('',#6340,#5099,#5100);
#4614=AXIS2_PLACEMENT_3D('',#6341,#5101,#5102);
#4615=AXIS2_PLACEMENT_3D('',#6343,#5103,#5104);
#4616=AXIS2_PLACEMENT_3D('',#6344,#5105,#5106);
#4617=AXIS2_PLACEMENT_3D('',#6346,#5107,#5108);
#4618=AXIS2_PLACEMENT_3D('',#6349,#5110,#5111);
#4619=AXIS2_PLACEMENT_3D('',#6350,#5112,#5113);
#4620=AXIS2_PLACEMENT_3D('',#6355,#5115,#5116);
#4621=AXIS2_PLACEMENT_3D('',#6359,#5118,#5119);
#4622=AXIS2_PLACEMENT_3D('',#6363,#5121,#5122);
#4623=AXIS2_PLACEMENT_3D('',#6366,#5124,#5125);
#4624=AXIS2_PLACEMENT_3D('',#6367,#5126,#5127);
#4625=AXIS2_PLACEMENT_3D('',#6369,#5128,#5129);
#4626=AXIS2_PLACEMENT_3D('',#6371,#5131,#5132);
#4627=AXIS2_PLACEMENT_3D('',#6373,#5133,#5134);
#4628=AXIS2_PLACEMENT_3D('',#6376,#5136,#5137);
#4629=AXIS2_PLACEMENT_3D('',#6377,#5138,#5139);
#4630=AXIS2_PLACEMENT_3D('',#6382,#5141,#5142);
#4631=AXIS2_PLACEMENT_3D('',#6386,#5144,#5145);
#4632=AXIS2_PLACEMENT_3D('',#6390,#5147,#5148);
#4633=AXIS2_PLACEMENT_3D('',#6393,#5150,#5151);
#4634=AXIS2_PLACEMENT_3D('',#6394,#5152,#5153);
#4635=AXIS2_PLACEMENT_3D('',#6397,#5155,#5156);
#4636=AXIS2_PLACEMENT_3D('',#6398,#5157,#5158);
#4637=AXIS2_PLACEMENT_3D('',#6404,#5162,#5163);
#4638=AXIS2_PLACEMENT_3D('',#6407,#5165,#5166);
#4639=AXIS2_PLACEMENT_3D('',#6408,#5167,#5168);
#4640=AXIS2_PLACEMENT_3D('',#6412,#5171,#5172);
#4641=AXIS2_PLACEMENT_3D('',#6415,#5174,#5175);
#4642=AXIS2_PLACEMENT_3D('',#6416,#5176,#5177);
#4643=AXIS2_PLACEMENT_3D('',#6420,#5180,#5181);
#4644=AXIS2_PLACEMENT_3D('',#6423,#5183,#5184);
#4645=AXIS2_PLACEMENT_3D('',#6424,#5185,#5186);
#4646=AXIS2_PLACEMENT_3D('',#6428,#5189,#5190);
#4647=AXIS2_PLACEMENT_3D('',#6429,#5191,#5192);
#4648=AXIS2_PLACEMENT_3D('',#6430,#5193,#5194);
#4649=AXIS2_PLACEMENT_3D('',#6434,#5196,#5197);
#4650=AXIS2_PLACEMENT_3D('',#6436,#5199,#5200);
#4651=AXIS2_PLACEMENT_3D('',#6440,#5203,#5204);
#4652=AXIS2_PLACEMENT_3D('',#6444,#5207,#5208);
#4653=AXIS2_PLACEMENT_3D('',#6445,#5209,#5210);
#4654=AXIS2_PLACEMENT_3D('',#6447,#5212,#5213);
#4655=AXIS2_PLACEMENT_3D('',#6452,#5217,#5218);
#4656=AXIS2_PLACEMENT_3D('',#6455,#5220,#5221);
#4657=AXIS2_PLACEMENT_3D('',#6456,#5222,#5223);
#4658=AXIS2_PLACEMENT_3D('',#6460,#5226,#5227);
#4659=AXIS2_PLACEMENT_3D('',#6463,#5229,#5230);
#4660=AXIS2_PLACEMENT_3D('',#6464,#5231,#5232);
#4661=AXIS2_PLACEMENT_3D('',#6467,#5235,#5236);
#4662=AXIS2_PLACEMENT_3D('',#6469,#5238,#5239);
#4663=AXIS2_PLACEMENT_3D('',#6471,#5241,#5242);
#4664=AXIS2_PLACEMENT_3D('',#6472,#5243,#5244);
#4665=AXIS2_PLACEMENT_3D('',#6475,#5247,#5248);
#4666=AXIS2_PLACEMENT_3D('',#6477,#5250,#5251);
#4667=AXIS2_PLACEMENT_3D('',#6479,#5253,#5254);
#4668=AXIS2_PLACEMENT_3D('',#6480,#5255,#5256);
#4669=AXIS2_PLACEMENT_3D('',#6483,#5258,#5259);
#4670=AXIS2_PLACEMENT_3D('',#6484,#5260,#5261);
#4671=AXIS2_PLACEMENT_3D('',#6485,#5262,#5263);
#4672=AXIS2_PLACEMENT_3D('',#6487,#5264,#5265);
#4673=AXIS2_PLACEMENT_3D('',#6488,#5266,#5267);
#4674=AXIS2_PLACEMENT_3D('',#6491,#5269,#5270);
#4675=AXIS2_PLACEMENT_3D('',#6492,#5271,#5272);
#4676=AXIS2_PLACEMENT_3D('',#6493,#5273,#5274);
#4677=AXIS2_PLACEMENT_3D('',#6494,#5275,#5276);
#4678=AXIS2_PLACEMENT_3D('',#6495,#5277,#5278);
#4679=AXIS2_PLACEMENT_3D('',#6497,#5279,#5280);
#4680=AXIS2_PLACEMENT_3D('',#6500,#5282,#5283);
#4681=AXIS2_PLACEMENT_3D('',#6501,#5284,#5285);
#4682=AXIS2_PLACEMENT_3D('',#6503,#5286,#5287);
#4683=AXIS2_PLACEMENT_3D('',#6506,#5289,#5290);
#4684=AXIS2_PLACEMENT_3D('',#6507,#5291,#5292);
#4685=AXIS2_PLACEMENT_3D('',#6509,#5294,#5295);
#4686=AXIS2_PLACEMENT_3D('',#6511,#5296,#5297);
#4687=AXIS2_PLACEMENT_3D('',#6512,#5298,#5299);
#4688=AXIS2_PLACEMENT_3D('',#6514,#5300,#5301);
#4689=AXIS2_PLACEMENT_3D('',#6516,#5303,#5304);
#4690=AXIS2_PLACEMENT_3D('',#6518,#5305,#5306);
#4691=AXIS2_PLACEMENT_3D('',#6520,#5308,#5309);
#4692=AXIS2_PLACEMENT_3D('',#6522,#5310,#5311);
#4693=AXIS2_PLACEMENT_3D('',#6524,#5313,#5314);
#4694=AXIS2_PLACEMENT_3D('',#6526,#5315,#5316);
#4695=AXIS2_PLACEMENT_3D('',#6527,#5317,#5318);
#4696=AXIS2_PLACEMENT_3D('',#6529,#5319,#5320);
#4697=AXIS2_PLACEMENT_3D('',#6531,#5322,#5323);
#4698=AXIS2_PLACEMENT_3D('',#6533,#5324,#5325);
#4699=AXIS2_PLACEMENT_3D('',#6535,#5327,#5328);
#4700=AXIS2_PLACEMENT_3D('',#6536,#5329,#5330);
#4701=AXIS2_PLACEMENT_3D('',#6537,#5331,#5332);
#4702=AXIS2_PLACEMENT_3D('',#6539,#5333,#5334);
#4703=AXIS2_PLACEMENT_3D('',#6542,#5336,#5337);
#4704=AXIS2_PLACEMENT_3D('',#6543,#5338,#5339);
#4705=AXIS2_PLACEMENT_3D('',#6545,#5340,#5341);
#4706=AXIS2_PLACEMENT_3D('',#6546,#5342,#5343);
#4707=AXIS2_PLACEMENT_3D('',#6549,#5345,#5346);
#4708=AXIS2_PLACEMENT_3D('',#6550,#5347,#5348);
#4709=AXIS2_PLACEMENT_3D('',#6552,#5349,#5350);
#4710=AXIS2_PLACEMENT_3D('',#6553,#5351,#5352);
#4711=AXIS2_PLACEMENT_3D('',#6555,#5353,#5354);
#4712=AXIS2_PLACEMENT_3D('',#6557,#5356,#5357);
#4713=AXIS2_PLACEMENT_3D('',#6559,#5358,#5359);
#4714=AXIS2_PLACEMENT_3D('',#6561,#5361,#5362);
#4715=AXIS2_PLACEMENT_3D('',#6563,#5363,#5364);
#4716=AXIS2_PLACEMENT_3D('',#6565,#5366,#5367);
#4717=AXIS2_PLACEMENT_3D('',#6567,#5368,#5369);
#4718=AXIS2_PLACEMENT_3D('',#6568,#5370,#5371);
#4719=AXIS2_PLACEMENT_3D('',#6571,#5373,#5374);
#4720=AXIS2_PLACEMENT_3D('',#6572,#5375,#5376);
#4721=AXIS2_PLACEMENT_3D('',#6574,#5377,#5378);
#4722=AXIS2_PLACEMENT_3D('',#6575,#5379,#5380);
#4723=AXIS2_PLACEMENT_3D('',#6577,#5381,#5382);
#4724=AXIS2_PLACEMENT_3D('',#6579,#5384,#5385);
#4725=AXIS2_PLACEMENT_3D('',#6581,#5386,#5387);
#4726=AXIS2_PLACEMENT_3D('',#6582,#5388,#5389);
#4727=AXIS2_PLACEMENT_3D('',#6585,#5391,#5392);
#4728=AXIS2_PLACEMENT_3D('',#6586,#5393,#5394);
#4729=AXIS2_PLACEMENT_3D('',#6589,#5396,#5397);
#4730=AXIS2_PLACEMENT_3D('',#6590,#5398,#5399);
#4731=AXIS2_PLACEMENT_3D('',#6593,#5401,#5402);
#4732=AXIS2_PLACEMENT_3D('',#6594,#5403,#5404);
#4733=AXIS2_PLACEMENT_3D('',#6595,#5405,#5406);
#4734=AXIS2_PLACEMENT_3D('',#6596,#5407,#5408);
#4735=AXIS2_PLACEMENT_3D('',#6598,#5409,#5410);
#4736=AXIS2_PLACEMENT_3D('',#6601,#5412,#5413);
#4737=AXIS2_PLACEMENT_3D('',#6602,#5414,#5415);
#4738=AXIS2_PLACEMENT_3D('',#6604,#5416,#5417);
#4739=AXIS2_PLACEMENT_3D('',#6605,#5418,#5419);
#4740=AXIS2_PLACEMENT_3D('',#6607,#5420,#5421);
#4741=AXIS2_PLACEMENT_3D('',#6609,#5423,#5424);
#4742=AXIS2_PLACEMENT_3D('',#6610,#5425,#5426);
#4743=AXIS2_PLACEMENT_3D('',#6611,#5427,#5428);
#4744=AXIS2_PLACEMENT_3D('',#6624,#5431,#5432);
#4745=AXIS2_PLACEMENT_3D('',#6638,#5436,#5437);
#4746=AXIS2_PLACEMENT_3D('',#6651,#5440,#5441);
#4747=AXIS2_PLACEMENT_3D('',#6665,#5445,#5446);
#4748=AXIS2_PLACEMENT_3D('',#6678,#5449,#5450);
#4749=AXIS2_PLACEMENT_3D('',#6692,#5454,#5455);
#4750=AXIS2_PLACEMENT_3D('',#6705,#5458,#5459);
#4751=AXIS2_PLACEMENT_3D('',#6719,#5463,#5464);
#4752=AXIS2_PLACEMENT_3D('',#6731,#5466,#5467);
#4753=AXIS2_PLACEMENT_3D('',#6733,#5468,#5469);
#4754=AXIS2_PLACEMENT_3D('',#6738,#5470,#5471);
#4755=AXIS2_PLACEMENT_3D('',#6739,#5472,#5473);
#4756=AXIS2_PLACEMENT_3D('',#6740,#5474,#5475);
#4757=AXIS2_PLACEMENT_3D('',#6747,#5476,#5477);
#4758=AXIS2_PLACEMENT_3D('',#6752,#5478,#5479);
#4759=AXIS2_PLACEMENT_3D('',#6754,#5481,#5482);
#4760=AXIS2_PLACEMENT_3D('',#6761,#5484,#5485);
#4761=AXIS2_PLACEMENT_3D('',#6763,#5486,#5487);
#4762=AXIS2_PLACEMENT_3D('',#6764,#5488,#5489);
#4763=AXIS2_PLACEMENT_3D('',#6766,#5490,#5491);
#4764=AXIS2_PLACEMENT_3D('',#6771,#5492,#5493);
#4765=AXIS2_PLACEMENT_3D('',#6778,#5495,#5496);
#4766=AXIS2_PLACEMENT_3D('',#6779,#5497,#5498);
#4767=AXIS2_PLACEMENT_3D('',#6780,#5499,#5500);
#4768=AXIS2_PLACEMENT_3D('',#6781,#5501,#5502);
#4769=AXIS2_PLACEMENT_3D('',#6782,#5503,#5504);
#4770=AXIS2_PLACEMENT_3D('',#6783,#5505,#5506);
#4771=AXIS2_PLACEMENT_3D('',#6784,#5507,#5508);
#4772=AXIS2_PLACEMENT_3D('',#6785,#5509,#5510);
#4773=AXIS2_PLACEMENT_3D('',#6804,#5511,#5512);
#4774=AXIS2_PLACEMENT_3D('',#6805,#5513,#5514);
#4775=AXIS2_PLACEMENT_3D('',#6806,#5515,#5516);
#4776=AXIS2_PLACEMENT_3D('',#6807,#5517,#5518);
#4777=AXIS2_PLACEMENT_3D('',#6809,#5519,#5520);
#4778=AXIS2_PLACEMENT_3D('',#6811,#5521,#5522);
#4779=AXIS2_PLACEMENT_3D('',#6813,#5523,#5524);
#4780=AXIS2_PLACEMENT_3D('',#6814,#5525,#5526);
#4781=AXIS2_PLACEMENT_3D('',#6815,#5527,#5528);
#4782=AXIS2_PLACEMENT_3D('',#6816,#5529,#5530);
#4783=AXIS2_PLACEMENT_3D('',#6828,#5531,#5532);
#4784=AXIS2_PLACEMENT_3D('',#6829,#5533,#5534);
#4785=AXIS2_PLACEMENT_3D('',#6830,#5535,#5536);
#4786=AXIS2_PLACEMENT_3D('',#6850,#5537,#5538);
#4787=AXIS2_PLACEMENT_3D('',#6854,#5540,#5541);
#4788=AXIS2_PLACEMENT_3D('',#6871,#5542,#5543);
#4789=AXIS2_PLACEMENT_3D('',#6897,#5544,#5545);
#4790=AXIS2_PLACEMENT_3D('',#6898,#5546,#5547);
#4791=AXIS2_PLACEMENT_3D('',#6899,#5548,#5549);
#4792=AXIS2_PLACEMENT_3D('',#6900,#5550,#5551);
#4793=AXIS2_PLACEMENT_3D('',#6901,#5552,#5553);
#4794=AXIS2_PLACEMENT_3D('',#6902,#5554,#5555);
#4795=AXIS2_PLACEMENT_3D('',#6904,#5556,#5557);
#4796=AXIS2_PLACEMENT_3D('',#6907,#5559,#5560);
#4797=AXIS2_PLACEMENT_3D('',#6908,#5561,#5562);
#4798=AXIS2_PLACEMENT_3D('',#6909,#5563,#5564);
#4799=AXIS2_PLACEMENT_3D('',#6911,#5565,#5566);
#4800=AXIS2_PLACEMENT_3D('',#6913,#5567,#5568);
#4801=AXIS2_PLACEMENT_3D('',#6914,#5569,#5570);
#4802=AXIS2_PLACEMENT_3D('',#6916,#5572,#5573);
#4803=AXIS2_PLACEMENT_3D('',#6918,#5575,#5576);
#4804=AXIS2_PLACEMENT_3D('',#6920,#5578,#5579);
#4805=AXIS2_PLACEMENT_3D('',#6922,#5581,#5582);
#4806=AXIS2_PLACEMENT_3D('',#6924,#5584,#5585);
#4807=AXIS2_PLACEMENT_3D('',#6925,#5586,#5587);
#4808=AXIS2_PLACEMENT_3D('',#6941,#5589,#5590);
#4809=AXIS2_PLACEMENT_3D('',#6949,#5591,#5592);
#4810=AXIS2_PLACEMENT_3D('',#6997,#5594,#5595);
#4811=AXIS2_PLACEMENT_3D('',#7045,#5597,#5598);
#4812=AXIS2_PLACEMENT_3D('',#7093,#5600,#5601);
#4813=AXIS2_PLACEMENT_3D('',#7147,#5603,#5604);
#4814=AXIS2_PLACEMENT_3D('',#7195,#5606,#5607);
#4815=AXIS2_PLACEMENT_3D('',#7209,#5609,#5610);
#4816=AXIS2_PLACEMENT_3D('',#7217,#5611,#5612);
#4817=AXIS2_PLACEMENT_3D('',#7242,#5614,#5615);
#4818=AXIS2_PLACEMENT_3D('',#7267,#5617,#5618);
#4819=AXIS2_PLACEMENT_3D('',#7291,#5620,#5621);
#4820=AXIS2_PLACEMENT_3D('',#7315,#5623,#5624);
#4821=AXIS2_PLACEMENT_3D('',#7394,#5625,#5626);
#4822=AXIS2_PLACEMENT_3D('',#7396,#5627,#5628);
#4823=AXIS2_PLACEMENT_3D('',#7719,#5629,#5630);
#4824=AXIS2_PLACEMENT_3D('',#7721,#5631,#5632);
#4825=AXIS2_PLACEMENT_3D('',#7722,#5633,#5634);
#4826=AXIS2_PLACEMENT_3D('',#7797,#5635,#5636);
#4827=AXIS2_PLACEMENT_3D('',#7798,#5637,#5638);
#4828=AXIS2_PLACEMENT_3D('',#7967,#5639,#5640);
#4829=AXIS2_PLACEMENT_3D('',#7976,#5645,#5646);
#4830=AXIS2_PLACEMENT_3D('',#7982,#5650,#5651);
#4831=AXIS2_PLACEMENT_3D('',#7988,#5655,#5656);
#4832=AXIS2_PLACEMENT_3D('',#7994,#5660,#5661);
#4833=AXIS2_PLACEMENT_3D('',#8000,#5665,#5666);
#4834=AXIS2_PLACEMENT_3D('',#8003,#5669,#5670);
#4835=AXIS2_PLACEMENT_3D('',#8004,#5671,#5672);
#4836=AXIS2_PLACEMENT_3D('',#8006,#5673,#5674);
#4837=AXIS2_PLACEMENT_3D('',#8007,#5675,#5676);
#4838=AXIS2_PLACEMENT_3D('',#8009,#5678,#5679);
#4839=AXIS2_PLACEMENT_3D('',#8010,#5680,#5681);
#4840=AXIS2_PLACEMENT_3D('',#8011,#5682,#5683);
#4841=AXIS2_PLACEMENT_3D('',#8013,#5684,#5685);
#4842=AXIS2_PLACEMENT_3D('',#8015,#5687,#5688);
#4843=AXIS2_PLACEMENT_3D('',#8016,#5689,#5690);
#4844=AXIS2_PLACEMENT_3D('',#8017,#5691,#5692);
#4845=AXIS2_PLACEMENT_3D('',#8033,#5694,#5695);
#4846=AXIS2_PLACEMENT_3D('',#8041,#5696,#5697);
#4847=AXIS2_PLACEMENT_3D('',#8089,#5699,#5700);
#4848=AXIS2_PLACEMENT_3D('',#8140,#5702,#5703);
#4849=AXIS2_PLACEMENT_3D('',#8191,#5705,#5706);
#4850=AXIS2_PLACEMENT_3D('',#8239,#5708,#5709);
#4851=AXIS2_PLACEMENT_3D('',#8251,#5711,#5712);
#4852=AXIS2_PLACEMENT_3D('',#8256,#5713,#5714);
#4853=AXIS2_PLACEMENT_3D('',#8281,#5716,#5717);
#4854=AXIS2_PLACEMENT_3D('',#8305,#5719,#5720);
#4855=AXIS2_PLACEMENT_3D('',#8331,#5722,#5723);
#4856=AXIS2_PLACEMENT_3D('',#8688,#5725,#5726);
#4857=AXIS2_PLACEMENT_3D('',#8690,#5727,#5728);
#4858=AXIS2_PLACEMENT_3D('',#8691,#5729,#5730);
#4859=AXIS2_PLACEMENT_3D('',#8775,#5731,#5732);
#4860=AXIS2_PLACEMENT_3D('',#8776,#5733,#5734);
#4861=AXIS2_PLACEMENT_3D('',#9023,#5735,#5736);
#4862=AXIS2_PLACEMENT_3D('',#9032,#5741,#5742);
#4863=AXIS2_PLACEMENT_3D('',#9041,#5747,#5748);
#4864=AXIS2_PLACEMENT_3D('',#9042,#5749,#5750);
#4865=AXIS2_PLACEMENT_3D('',#9043,#5751,#5752);
#4866=AXIS2_PLACEMENT_3D('',#9045,#5753,#5754);
#4867=AXIS2_PLACEMENT_3D('',#9046,#5755,#5756);
#4868=AXIS2_PLACEMENT_3D('',#9047,#5757,#5758);
#4869=AXIS2_PLACEMENT_3D('',#9048,#5759,#5760);
#4870=AXIS2_PLACEMENT_3D('',#9051,#5761,#5762);
#4871=AXIS2_PLACEMENT_3D('',#9057,#5766,#5767);
#4872=AXIS2_PLACEMENT_3D('',#9059,#5768,#5769);
#4873=AXIS2_PLACEMENT_3D('',#9063,#5772,#5773);
#4874=AXIS2_PLACEMENT_3D('',#9065,#5774,#5775);
#4875=AXIS2_PLACEMENT_3D('',#9069,#5778,#5779);
#4876=AXIS2_PLACEMENT_3D('',#9071,#5780,#5781);
#4877=AXIS2_PLACEMENT_3D('',#9075,#5784,#5785);
#4878=AXIS2_PLACEMENT_3D('',#9077,#5786,#5787);
#4879=AXIS2_PLACEMENT_3D('',#9081,#5790,#5791);
#4880=AXIS2_PLACEMENT_3D('',#9082,#5792,#5793);
#4881=AXIS2_PLACEMENT_3D('',#9084,#5795,#5796);
#4882=AXIS2_PLACEMENT_3D('',#9085,#5797,#5798);
#4883=AXIS2_PLACEMENT_3D('',#9088,#5799,#5800);
#4884=AXIS2_PLACEMENT_3D('',#9090,#5801,#5802);
#4885=AXIS2_PLACEMENT_3D('',#9092,#5803,#5804);
#4886=AXIS2_PLACEMENT_3D('',#9093,#5805,#5806);
#4887=AXIS2_PLACEMENT_3D('',#9095,#5807,#5808);
#4888=AXIS2_PLACEMENT_3D('',#9096,#5809,#5810);
#4889=AXIS2_PLACEMENT_3D('',#9098,#5811,#5812);
#4890=AXIS2_PLACEMENT_3D('',#9099,#5813,#5814);
#4891=AXIS2_PLACEMENT_3D('',#9101,#5816,#5817);
#4892=AXIS2_PLACEMENT_3D('',#9102,#5818,#5819);
#4893=AXIS2_PLACEMENT_3D('',#9103,#5820,#5821);
#4894=AXIS2_PLACEMENT_3D('',#9104,#5822,#5823);
#4895=AXIS2_PLACEMENT_3D('',#9105,#5824,#5825);
#4896=AXIS2_PLACEMENT_3D('',#9106,#5826,#5827);
#4897=AXIS2_PLACEMENT_3D('',#9108,#5829,#5830);
#4898=AXIS2_PLACEMENT_3D('',#9109,#5831,#5832);
#4899=AXIS2_PLACEMENT_3D('',#9111,#5833,#5834);
#4900=AXIS2_PLACEMENT_3D('',#9115,#5836,#5837);
#4901=AXIS2_PLACEMENT_3D('',#9116,#5838,#5839);
#4902=AXIS2_PLACEMENT_3D('',#9117,#5840,#5841);
#4903=AXIS2_PLACEMENT_3D('',#9120,#5843,#5844);
#4904=AXIS2_PLACEMENT_3D('',#9121,#5845,#5846);
#4905=AXIS2_PLACEMENT_3D('',#9122,#5847,#5848);
#4906=AXIS2_PLACEMENT_3D('',#9125,#5849,#5850);
#4907=AXIS2_PLACEMENT_3D('',#9126,#5851,#5852);
#4908=AXIS2_PLACEMENT_3D('',#9129,#5854,#5855);
#4909=AXIS2_PLACEMENT_3D('',#9130,#5856,#5857);
#4910=AXIS2_PLACEMENT_3D('',#9131,#5858,#5859);
#4911=AXIS2_PLACEMENT_3D('',#9133,#5860,#5861);
#4912=AXIS2_PLACEMENT_3D('',#9135,#5863,#5864);
#4913=AXIS2_PLACEMENT_3D('',#9213,#5866,#5867);
#4914=AXIS2_PLACEMENT_3D('',#9215,#5869,#5870);
#4915=AXIS2_PLACEMENT_3D('',#9216,#5871,#5872);
#4916=AXIS2_PLACEMENT_3D('',#9225,#5877,#5878);
#4917=AXIS2_PLACEMENT_3D('',#9227,#5879,#5880);
#4918=AXIS2_PLACEMENT_3D('',#9230,#5882,#5883);
#4919=AXIS2_PLACEMENT_3D('',#9231,#5884,#5885);
#4920=AXIS2_PLACEMENT_3D('',#9237,#5889,#5890);
#4921=AXIS2_PLACEMENT_3D('',#9239,#5891,#5892);
#4922=AXIS2_PLACEMENT_3D('',#9242,#5894,#5895);
#4923=AXIS2_PLACEMENT_3D('',#9243,#5896,#5897);
#4924=AXIS2_PLACEMENT_3D('',#9249,#5901,#5902);
#4925=AXIS2_PLACEMENT_3D('',#9251,#5903,#5904);
#4926=AXIS2_PLACEMENT_3D('',#9254,#5906,#5907);
#4927=AXIS2_PLACEMENT_3D('',#9255,#5908,#5909);
#4928=AXIS2_PLACEMENT_3D('',#9261,#5913,#5914);
#4929=AXIS2_PLACEMENT_3D('',#9263,#5915,#5916);
#4930=AXIS2_PLACEMENT_3D('',#9266,#5918,#5919);
#4931=AXIS2_PLACEMENT_3D('',#9267,#5920,#5921);
#4932=AXIS2_PLACEMENT_3D('',#9271,#5923,#5924);
#4933=AXIS2_PLACEMENT_3D('',#9272,#5925,#5926);
#4934=AXIS2_PLACEMENT_3D('',#9273,#5927,#5928);
#4935=AXIS2_PLACEMENT_3D('',#9275,#5929,#5930);
#4936=AXIS2_PLACEMENT_3D('',#9278,#5932,#5933);
#4937=AXIS2_PLACEMENT_3D('',#9279,#5934,#5935);
#4938=AXIS2_PLACEMENT_3D('',#9285,#5939,#5940);
#4939=AXIS2_PLACEMENT_3D('',#9287,#5941,#5942);
#4940=AXIS2_PLACEMENT_3D('',#9290,#5944,#5945);
#4941=AXIS2_PLACEMENT_3D('',#9291,#5946,#5947);
#4942=AXIS2_PLACEMENT_3D('',#9297,#5951,#5952);
#4943=AXIS2_PLACEMENT_3D('',#9301,#5954,#5955);
#4944=AXIS2_PLACEMENT_3D('',#9302,#5956,#5957);
#4945=AXIS2_PLACEMENT_3D('',#9303,#5958,#5959);
#4946=AXIS2_PLACEMENT_3D('',#9309,#5963,#5964);
#4947=AXIS2_PLACEMENT_3D('',#9311,#5965,#5966);
#4948=AXIS2_PLACEMENT_3D('',#9314,#5968,#5969);
#4949=AXIS2_PLACEMENT_3D('',#9315,#5970,#5971);
#4950=AXIS2_PLACEMENT_3D('',#9321,#5975,#5976);
#4951=AXIS2_PLACEMENT_3D('',#9323,#5977,#5978);
#4952=AXIS2_PLACEMENT_3D('',#9326,#5980,#5981);
#4953=AXIS2_PLACEMENT_3D('',#9327,#5982,#5983);
#4954=AXIS2_PLACEMENT_3D('',#9329,#5984,#5985);
#4955=AXIS2_PLACEMENT_3D('',#9332,#5987,#5988);
#4956=AXIS2_PLACEMENT_3D('',#9333,#5989,#5990);
#4957=AXIS2_PLACEMENT_3D('',#9334,#5991,#5992);
#4958=AXIS2_PLACEMENT_3D('',#9335,#5993,#5994);
#4959=AXIS2_PLACEMENT_3D('',#9336,#5995,#5996);
#4960=AXIS2_PLACEMENT_3D('',#9339,#5998,#5999);
#4961=AXIS2_PLACEMENT_3D('',#9340,#6000,#6001);
#4962=AXIS2_PLACEMENT_3D('',#9343,#6004,#6005);
#4963=AXIS2_PLACEMENT_3D('',#9345,#6007,#6008);
#4964=AXIS2_PLACEMENT_3D('',#9347,#6010,#6011);
#4965=AXIS2_PLACEMENT_3D('',#9349,#6013,#6014);
#4966=AXIS2_PLACEMENT_3D('',#9350,#6015,#6016);
#4967=AXIS2_PLACEMENT_3D('',#9353,#6018,#6019);
#4968=AXIS2_PLACEMENT_3D('',#9354,#6020,#6021);
#4969=AXIS2_PLACEMENT_3D('',#9356,#6023,#6024);
#4970=AXIS2_PLACEMENT_3D('',#9358,#6026,#6027);
#4971=AXIS2_PLACEMENT_3D('',#9360,#6029,#6030);
#4972=AXIS2_PLACEMENT_3D('',#9363,#6032,#6033);
#4973=AXIS2_PLACEMENT_3D('',#9364,#6034,#6035);
#4974=AXIS2_PLACEMENT_3D('',#9367,#6037,#6038);
#4975=AXIS2_PLACEMENT_3D('',#9368,#6039,#6040);
#4976=AXIS2_PLACEMENT_3D('',#9369,#6041,#6042);
#4977=AXIS2_PLACEMENT_3D('',#9370,#6043,#6044);
#4978=AXIS2_PLACEMENT_3D('',#9371,#6045,#6046);
#4979=AXIS2_PLACEMENT_3D('',#9373,#6047,#6048);
#4980=AXIS2_PLACEMENT_3D('',#9376,#6050,#6051);
#4981=AXIS2_PLACEMENT_3D('',#9377,#6052,#6053);
#4982=AXIS2_PLACEMENT_3D('',#9379,#6054,#6055);
#4983=AXIS2_PLACEMENT_3D('',#9380,#6056,#6057);
#4984=AXIS2_PLACEMENT_3D('',#9382,#6058,#6059);
#4985=AXIS2_PLACEMENT_3D('',#9384,#6061,#6062);
#4986=AXIS2_PLACEMENT_3D('',#9386,#6063,#6064);
#4987=AXIS2_PLACEMENT_3D('',#9387,#6065,#6066);
#4988=AXIS2_PLACEMENT_3D('',#9389,#6067,#6068);
#4989=AXIS2_PLACEMENT_3D('',#9391,#6070,#6071);
#4990=AXIS2_PLACEMENT_3D('',#9392,#6072,#6073);
#4991=AXIS2_PLACEMENT_3D('',#9393,#6074,#6075);
#4992=AXIS2_PLACEMENT_3D('',#9409,#6077,#6078);
#4993=AXIS2_PLACEMENT_3D('',#9417,#6079,#6080);
#4994=AXIS2_PLACEMENT_3D('',#9465,#6082,#6083);
#4995=AXIS2_PLACEMENT_3D('',#9513,#6085,#6086);
#4996=AXIS2_PLACEMENT_3D('',#9561,#6088,#6089);
#4997=AXIS2_PLACEMENT_3D('',#9615,#6091,#6092);
#4998=AXIS2_PLACEMENT_3D('',#9663,#6094,#6095);
#4999=AXIS2_PLACEMENT_3D('',#9711,#6097,#6098);
#5000=AXIS2_PLACEMENT_3D('',#9765,#6100,#6101);
#5001=AXIS2_PLACEMENT_3D('',#9813,#6103,#6104);
#5002=AXIS2_PLACEMENT_3D('',#9861,#6106,#6107);
#5003=AXIS2_PLACEMENT_3D('',#9909,#6109,#6110);
#5004=AXIS2_PLACEMENT_3D('',#9963,#6112,#6113);
#5005=AXIS2_PLACEMENT_3D('',#9975,#6115,#6116);
#5006=AXIS2_PLACEMENT_3D('',#9981,#6117,#6118);
#5007=AXIS2_PLACEMENT_3D('',#10006,#6120,#6121);
#5008=AXIS2_PLACEMENT_3D('',#10031,#6123,#6124);
#5009=AXIS2_PLACEMENT_3D('',#10055,#6126,#6127);
#5010=AXIS2_PLACEMENT_3D('',#10079,#6129,#6130);
#5011=AXIS2_PLACEMENT_3D('',#10104,#6132,#6133);
#5012=AXIS2_PLACEMENT_3D('',#10129,#6135,#6136);
#5013=AXIS2_PLACEMENT_3D('',#10153,#6138,#6139);
#5014=AXIS2_PLACEMENT_3D('',#10178,#6141,#6142);
#5015=AXIS2_PLACEMENT_3D('',#10203,#6144,#6145);
#5016=AXIS2_PLACEMENT_3D('',#10227,#6147,#6148);
#5017=AXIS2_PLACEMENT_3D('',#10754,#6150,#6151);
#5018=AXIS2_PLACEMENT_3D('',#10756,#6152,#6153);
#5019=AXIS2_PLACEMENT_3D('',#10757,#6154,#6155);
#5020=AXIS2_PLACEMENT_3D('',#10832,#6156,#6157);
#5021=AXIS2_PLACEMENT_3D('',#10833,#6158,#6159);
#5022=AXIS2_PLACEMENT_3D('',#11259,#6160,#6161);
#5023=AXIS2_PLACEMENT_3D('',#11268,#6166,#6167);
#5024=AXIS2_PLACEMENT_3D('',#11277,#6172,#6173);
#5025=AXIS2_PLACEMENT_3D('',#11286,#6178,#6179);
#5026=AXIS2_PLACEMENT_3D('',#11292,#6183,#6184);
#5027=AXIS2_PLACEMENT_3D('',#11298,#6188,#6189);
#5028=AXIS2_PLACEMENT_3D('',#11301,#6192,#6193);
#5029=AXIS2_PLACEMENT_3D('',#11307,#6197,#6198);
#5030=AXIS2_PLACEMENT_3D('',#11309,#6199,#6200);
#5031=AXIS2_PLACEMENT_3D('',#11318,#6206,#6207);
#5032=AXIS2_PLACEMENT_3D('',#11322,#6210,#6211);
#5033=AXIS2_PLACEMENT_3D('',#11324,#6213,#6214);
#5034=AXIS2_PLACEMENT_3D('',#11328,#6217,#6218);
#5035=AXIS2_PLACEMENT_3D('',#11332,#6221,#6222);
#5036=AXIS2_PLACEMENT_3D('',#11334,#6224,#6225);
#5037=AXIS2_PLACEMENT_3D('',#11335,#6226,#6227);
#5038=AXIS2_PLACEMENT_3D('',#11337,#6228,#6229);
#5039=AXIS2_PLACEMENT_3D('',#11338,#6230,#6231);
#5040=AXIS2_PLACEMENT_3D('',#11340,#6233,#6234);
#5041=AXIS2_PLACEMENT_3D('',#11341,#6235,#6236);
#5042=AXIS2_PLACEMENT_3D('',#11342,#6237,#6238);
#5043=AXIS2_PLACEMENT_3D('',#11344,#6239,#6240);
#5044=AXIS2_PLACEMENT_3D('',#11345,#6241,#6242);
#5045=AXIS2_PLACEMENT_3D('',#11347,#6243,#6244);
#5046=AXIS2_PLACEMENT_3D('',#11349,#6246,#6247);
#5047=AXIS2_PLACEMENT_3D('',#11351,#6249,#6250);
#5048=AXIS2_PLACEMENT_3D('',#11352,#6251,#6252);
#5049=AXIS2_PLACEMENT_3D('',#11354,#6253,#6254);
#5050=AXIS2_PLACEMENT_3D('',#11358,#6256,#6257);
#5051=AXIS2_PLACEMENT_3D('',#11359,#6258,#6259);
#5052=AXIS2_PLACEMENT_3D('',#11360,#6260,#6261);
#5053=AXIS2_PLACEMENT_3D('',#11363,#6262,#6263);
#5054=AXIS2_PLACEMENT_3D('',#11364,#6264,#6265);
#5055=AXIS2_PLACEMENT_3D('',#11366,#6267,#6268);
#5056=AXIS2_PLACEMENT_3D('',#11368,#6269,#6270);
#5057=AXIS2_PLACEMENT_3D('',#11369,#6271,#6272);
#5058=AXIS2_PLACEMENT_3D('',#11372,#6274,#6275);
#5059=AXIS2_PLACEMENT_3D('',#11373,#6276,#6277);
#5060=AXIS2_PLACEMENT_3D('',#11375,#6278,#6279);
#5061=AXIS2_PLACEMENT_3D('',#11376,#6280,#6281);
#5062=AXIS2_PLACEMENT_3D('',#11378,#6282,#6283);
#5063=AXIS2_PLACEMENT_3D('',#11380,#6285,#6286);
#5064=AXIS2_PLACEMENT_3D('',#11382,#6287,#6288);
#5065=AXIS2_PLACEMENT_3D('',#11384,#6290,#6291);
#5066=AXIS2_PLACEMENT_3D('',#11386,#6293,#6294);
#5067=AXIS2_PLACEMENT_3D('',#11387,#6295,#6296);
#5068=AXIS2_PLACEMENT_3D('',#11388,#6297,#6298);
#5069=AXIS2_PLACEMENT_3D('',#11389,#6299,#6300);
#5070=AXIS2_PLACEMENT_3D('',#11390,#6301,#6302);
#5071=AXIS2_PLACEMENT_3D('',#11391,#6303,#6304);
#5072=AXIS2_PLACEMENT_3D('',#11392,#6305,#6306);
#5073=AXIS2_PLACEMENT_3D('',#11393,#6307,#6308);
#5074=AXIS2_PLACEMENT_3D('',#11394,#6309,#6310);
#5075=AXIS2_PLACEMENT_3D('',#11395,#6311,#6312);
#5076=AXIS2_PLACEMENT_3D('',#11396,#6313,#6314);
#5077=AXIS2_PLACEMENT_3D('',#11397,#6315,#6316);
#5078=AXIS2_PLACEMENT_3D('',#11398,#6317,#6318);
#5079=AXIS2_PLACEMENT_3D('',#11399,#6319,#6320);
#5080=AXIS2_PLACEMENT_3D('',#11400,#6321,#6322);
#5081=AXIS2_PLACEMENT_3D('',#11401,#6323,#6324);
#5082=AXIS2_PLACEMENT_3D('',#11402,#6325,#6326);
#5083=DIRECTION('axis',(0.,0.,1.));
#5084=DIRECTION('refdir',(1.,0.,0.));
#5085=DIRECTION('axis',(0.,0.,1.));
#5086=DIRECTION('refdir',(1.,0.,0.));
#5087=DIRECTION('center_axis',(0.,1.,0.));
#5088=DIRECTION('ref_axis',(1.,0.,0.));
#5089=DIRECTION('center_axis',(0.,1.,0.));
#5090=DIRECTION('ref_axis',(1.,0.,0.));
#5091=DIRECTION('',(-0.707106781186547,0.707106781186548,-8.65956056235493E-17));
#5092=DIRECTION('center_axis',(0.,-1.,0.));
#5093=DIRECTION('ref_axis',(1.,0.,0.));
#5094=DIRECTION('center_axis',(0.,-1.,0.));
#5095=DIRECTION('ref_axis',(1.,0.,0.));
#5096=DIRECTION('',(0.,1.,0.));
#5097=DIRECTION('center_axis',(0.,1.,0.));
#5098=DIRECTION('ref_axis',(1.,0.,0.));
#5099=DIRECTION('center_axis',(0.,1.,0.));
#5100=DIRECTION('ref_axis',(1.,0.,0.));
#5101=DIRECTION('center_axis',(0.,1.,0.));
#5102=DIRECTION('ref_axis',(1.,0.,0.));
#5103=DIRECTION('center_axis',(0.,1.,0.));
#5104=DIRECTION('ref_axis',(1.,0.,0.));
#5105=DIRECTION('center_axis',(0.,0.,1.));
#5106=DIRECTION('ref_axis',(1.,0.,0.));
#5107=DIRECTION('center_axis',(0.,0.,1.));
#5108=DIRECTION('ref_axis',(1.,0.,0.));
#5109=DIRECTION('',(0.707106781186548,8.65956056235493E-17,-0.707106781186548));
#5110=DIRECTION('center_axis',(0.,0.,-1.));
#5111=DIRECTION('ref_axis',(1.,0.,0.));
#5112=DIRECTION('center_axis',(0.,0.,1.));
#5113=DIRECTION('ref_axis',(1.,0.,0.));
#5114=DIRECTION('',(-1.,0.,0.));
#5115=DIRECTION('center_axis',(0.,0.,-1.));
#5116=DIRECTION('ref_axis',(0.,-1.,0.));
#5117=DIRECTION('',(0.,-1.,0.));
#5118=DIRECTION('center_axis',(0.,0.,-1.));
#5119=DIRECTION('ref_axis',(1.,0.,0.));
#5120=DIRECTION('',(1.,0.,0.));
#5121=DIRECTION('center_axis',(0.,0.,-1.));
#5122=DIRECTION('ref_axis',(0.,1.,0.));
#5123=DIRECTION('',(0.,1.,0.));
#5124=DIRECTION('center_axis',(0.,0.,-1.));
#5125=DIRECTION('ref_axis',(-1.,0.,0.));
#5126=DIRECTION('center_axis',(0.,0.,1.));
#5127=DIRECTION('ref_axis',(1.,0.,0.));
#5128=DIRECTION('center_axis',(0.,0.,1.));
#5129=DIRECTION('ref_axis',(1.,0.,0.));
#5130=DIRECTION('',(0.,0.,1.));
#5131=DIRECTION('center_axis',(0.,0.,-1.));
#5132=DIRECTION('ref_axis',(1.,0.,0.));
#5133=DIRECTION('center_axis',(0.,0.,-1.));
#5134=DIRECTION('ref_axis',(1.,0.,0.));
#5135=DIRECTION('',(0.707106781186548,-8.65956056235493E-17,0.707106781186548));
#5136=DIRECTION('center_axis',(0.,0.,1.));
#5137=DIRECTION('ref_axis',(1.,0.,0.));
#5138=DIRECTION('center_axis',(0.,0.,1.));
#5139=DIRECTION('ref_axis',(1.,0.,0.));
#5140=DIRECTION('',(1.,0.,0.));
#5141=DIRECTION('center_axis',(0.,0.,1.));
#5142=DIRECTION('ref_axis',(-1.,0.,0.));
#5143=DIRECTION('',(0.,-1.,0.));
#5144=DIRECTION('center_axis',(0.,0.,1.));
#5145=DIRECTION('ref_axis',(0.,1.,0.));
#5146=DIRECTION('',(-1.,0.,0.));
#5147=DIRECTION('center_axis',(0.,0.,1.));
#5148=DIRECTION('ref_axis',(1.,0.,0.));
#5149=DIRECTION('',(0.,1.,0.));
#5150=DIRECTION('center_axis',(0.,0.,1.));
#5151=DIRECTION('ref_axis',(0.,-1.,0.));
#5152=DIRECTION('center_axis',(0.,0.,1.));
#5153=DIRECTION('ref_axis',(1.,0.,0.));
#5154=DIRECTION('',(0.,0.,1.));
#5155=DIRECTION('center_axis',(0.,0.,1.));
#5156=DIRECTION('ref_axis',(1.,0.,0.));
#5157=DIRECTION('center_axis',(0.,-0.707106781186547,-0.707106781186548));
#5158=DIRECTION('ref_axis',(-1.,0.,0.));
#5159=DIRECTION('',(0.,-0.707106781186548,0.707106781186547));
#5160=DIRECTION('',(-1.,0.,0.));
#5161=DIRECTION('',(0.,0.707106781186548,-0.707106781186547));
#5162=DIRECTION('center_axis',(0.,0.,1.));
#5163=DIRECTION('ref_axis',(0.,-1.,0.));
#5164=DIRECTION('',(0.707106781186548,0.,0.707106781186547));
#5165=DIRECTION('center_axis',(0.,0.,-1.));
#5166=DIRECTION('ref_axis',(0.,-1.,0.));
#5167=DIRECTION('center_axis',(0.707106781186547,0.,-0.707106781186548));
#5168=DIRECTION('ref_axis',(-0.707106781186548,0.,-0.707106781186547));
#5169=DIRECTION('',(0.707106781186548,0.,0.707106781186547));
#5170=DIRECTION('',(0.,-1.,0.));
#5171=DIRECTION('center_axis',(0.,0.,1.));
#5172=DIRECTION('ref_axis',(1.,0.,0.));
#5173=DIRECTION('',(0.,0.707106781186548,0.707106781186547));
#5174=DIRECTION('center_axis',(0.,0.,-1.));
#5175=DIRECTION('ref_axis',(1.,0.,0.));
#5176=DIRECTION('center_axis',(0.,0.707106781186547,-0.707106781186548));
#5177=DIRECTION('ref_axis',(-1.,0.,0.));
#5178=DIRECTION('',(0.,0.707106781186548,0.707106781186547));
#5179=DIRECTION('',(1.,0.,0.));
#5180=DIRECTION('center_axis',(0.,0.,1.));
#5181=DIRECTION('ref_axis',(0.,1.,0.));
#5182=DIRECTION('',(-0.707106781186548,0.,0.707106781186547));
#5183=DIRECTION('center_axis',(0.,0.,-1.));
#5184=DIRECTION('ref_axis',(0.,1.,0.));
#5185=DIRECTION('center_axis',(-0.707106781186547,0.,-0.707106781186548));
#5186=DIRECTION('ref_axis',(-0.707106781186548,0.,0.707106781186547));
#5187=DIRECTION('',(-0.707106781186548,0.,0.707106781186547));
#5188=DIRECTION('',(0.,1.,0.));
#5189=DIRECTION('center_axis',(0.,0.,1.));
#5190=DIRECTION('ref_axis',(-1.,0.,0.));
#5191=DIRECTION('center_axis',(0.,0.,-1.));
#5192=DIRECTION('ref_axis',(-1.,0.,0.));
#5193=DIRECTION('center_axis',(0.,0.,1.));
#5194=DIRECTION('ref_axis',(0.,1.,0.));
#5195=DIRECTION('',(0.,0.,1.));
#5196=DIRECTION('center_axis',(0.,0.,1.));
#5197=DIRECTION('ref_axis',(0.,1.,0.));
#5198=DIRECTION('',(0.,0.,1.));
#5199=DIRECTION('center_axis',(-1.,0.,0.));
#5200=DIRECTION('ref_axis',(0.,-1.,0.));
#5201=DIRECTION('',(0.,0.,1.));
#5202=DIRECTION('',(0.,-1.,0.));
#5203=DIRECTION('center_axis',(0.,0.,1.));
#5204=DIRECTION('ref_axis',(-1.,0.,0.));
#5205=DIRECTION('',(0.,0.,1.));
#5206=DIRECTION('',(0.,0.,1.));
#5207=DIRECTION('center_axis',(0.,0.,1.));
#5208=DIRECTION('ref_axis',(-1.,0.,0.));
#5209=DIRECTION('center_axis',(0.,-1.,0.));
#5210=DIRECTION('ref_axis',(1.,0.,0.));
#5211=DIRECTION('',(0.,0.,1.));
#5212=DIRECTION('center_axis',(0.,-0.707106781186548,0.707106781186548));
#5213=DIRECTION('ref_axis',(1.,0.,0.));
#5214=DIRECTION('',(0.,0.707106781186548,0.707106781186548));
#5215=DIRECTION('',(0.,-0.707106781186548,-0.707106781186548));
#5216=DIRECTION('',(1.,0.,0.));
#5217=DIRECTION('center_axis',(0.,0.,-1.));
#5218=DIRECTION('ref_axis',(0.,-1.,0.));
#5219=DIRECTION('',(-0.707106781186548,0.,0.707106781186548));
#5220=DIRECTION('center_axis',(0.,0.,1.));
#5221=DIRECTION('ref_axis',(0.,-1.,0.));
#5222=DIRECTION('center_axis',(0.707106781186548,0.,0.707106781186548));
#5223=DIRECTION('ref_axis',(0.707106781186548,0.,-0.707106781186548));
#5224=DIRECTION('',(-0.707106781186548,0.,0.707106781186548));
#5225=DIRECTION('',(0.,1.,0.));
#5226=DIRECTION('center_axis',(0.,0.,-1.));
#5227=DIRECTION('ref_axis',(1.,0.,0.));
#5228=DIRECTION('',(0.,-0.707106781186548,0.707106781186548));
#5229=DIRECTION('center_axis',(0.,0.,1.));
#5230=DIRECTION('ref_axis',(1.,0.,0.));
#5231=DIRECTION('center_axis',(0.,0.707106781186548,0.707106781186548));
#5232=DIRECTION('ref_axis',(1.,0.,0.));
#5233=DIRECTION('',(0.,-0.707106781186548,0.707106781186548));
#5234=DIRECTION('',(-1.,0.,0.));
#5235=DIRECTION('center_axis',(0.,0.,-1.));
#5236=DIRECTION('ref_axis',(0.,1.,0.));
#5237=DIRECTION('',(0.707106781186548,0.,0.707106781186548));
#5238=DIRECTION('center_axis',(-0.707106781186548,0.,0.707106781186548));
#5239=DIRECTION('ref_axis',(0.707106781186548,0.,0.707106781186548));
#5240=DIRECTION('',(0.707106781186548,0.,0.707106781186548));
#5241=DIRECTION('center_axis',(0.,0.,-1.));
#5242=DIRECTION('ref_axis',(-1.,0.,0.));
#5243=DIRECTION('center_axis',(0.,0.,1.));
#5244=DIRECTION('ref_axis',(1.,0.,0.));
#5245=DIRECTION('',(0.,0.,1.));
#5246=DIRECTION('',(0.,0.,1.));
#5247=DIRECTION('center_axis',(1.,0.,0.));
#5248=DIRECTION('ref_axis',(0.,1.,0.));
#5249=DIRECTION('',(0.,0.,1.));
#5250=DIRECTION('center_axis',(0.,0.,1.));
#5251=DIRECTION('ref_axis',(0.,-1.,0.));
#5252=DIRECTION('',(0.,0.,1.));
#5253=DIRECTION('center_axis',(0.,-1.,0.));
#5254=DIRECTION('ref_axis',(1.,0.,0.));
#5255=DIRECTION('center_axis',(0.,1.,0.));
#5256=DIRECTION('ref_axis',(1.,0.,0.));
#5257=DIRECTION('',(0.,1.,0.));
#5258=DIRECTION('center_axis',(0.,1.,0.));
#5259=DIRECTION('ref_axis',(1.,0.,0.));
#5260=DIRECTION('center_axis',(0.,1.,0.));
#5261=DIRECTION('ref_axis',(1.,0.,0.));
#5262=DIRECTION('center_axis',(0.,0.,1.));
#5263=DIRECTION('ref_axis',(1.,0.,0.));
#5264=DIRECTION('center_axis',(0.,0.,1.));
#5265=DIRECTION('ref_axis',(1.,0.,0.));
#5266=DIRECTION('center_axis',(0.,0.,1.));
#5267=DIRECTION('ref_axis',(1.,0.,0.));
#5268=DIRECTION('',(0.,0.,1.));
#5269=DIRECTION('center_axis',(0.,0.,1.));
#5270=DIRECTION('ref_axis',(1.,0.,0.));
#5271=DIRECTION('center_axis',(0.,0.,-1.));
#5272=DIRECTION('ref_axis',(-1.,0.,0.));
#5273=DIRECTION('center_axis',(0.,1.,0.));
#5274=DIRECTION('ref_axis',(-1.,0.,0.));
#5275=DIRECTION('axis',(0.,0.,1.));
#5276=DIRECTION('refdir',(1.,0.,0.));
#5277=DIRECTION('center_axis',(1.,0.,0.));
#5278=DIRECTION('ref_axis',(0.,1.,0.));
#5279=DIRECTION('center_axis',(1.,0.,0.));
#5280=DIRECTION('ref_axis',(0.,1.,0.));
#5281=DIRECTION('',(0.775435860081924,-0.631426343209568,-7.73274250108915E-17));
#5282=DIRECTION('center_axis',(-1.,0.,0.));
#5283=DIRECTION('ref_axis',(0.,1.,0.));
#5284=DIRECTION('center_axis',(-1.,0.,0.));
#5285=DIRECTION('ref_axis',(0.,1.,0.));
#5286=DIRECTION('center_axis',(1.,0.,0.));
#5287=DIRECTION('ref_axis',(0.,1.,0.));
#5288=DIRECTION('',(0.775435860081925,0.631426343209567,7.73274250108914E-17));
#5289=DIRECTION('center_axis',(-1.,0.,0.));
#5290=DIRECTION('ref_axis',(0.,1.,0.));
#5291=DIRECTION('center_axis',(1.,0.,0.));
#5292=DIRECTION('ref_axis',(0.,1.,0.));
#5293=DIRECTION('',(-1.,0.,0.));
#5294=DIRECTION('center_axis',(-1.,0.,0.));
#5295=DIRECTION('ref_axis',(0.,0.,1.));
#5296=DIRECTION('center_axis',(1.,0.,0.));
#5297=DIRECTION('ref_axis',(0.,0.,-1.));
#5298=DIRECTION('center_axis',(1.,0.,0.));
#5299=DIRECTION('ref_axis',(0.,1.,0.));
#5300=DIRECTION('center_axis',(1.,0.,0.));
#5301=DIRECTION('ref_axis',(0.,0.,-1.));
#5302=DIRECTION('',(-0.554700196225229,0.832050294337844,1.01896772969045E-16));
#5303=DIRECTION('center_axis',(1.,0.,0.));
#5304=DIRECTION('ref_axis',(0.,1.,0.));
#5305=DIRECTION('center_axis',(1.,0.,0.));
#5306=DIRECTION('ref_axis',(0.,0.,-1.));
#5307=DIRECTION('',(-1.,0.,0.));
#5308=DIRECTION('center_axis',(-1.,0.,0.));
#5309=DIRECTION('ref_axis',(0.,1.,0.));
#5310=DIRECTION('center_axis',(1.,0.,0.));
#5311=DIRECTION('ref_axis',(0.,0.,-1.));
#5312=DIRECTION('',(-0.707106781186547,-0.707106781186548,-8.65956056235494E-17));
#5313=DIRECTION('center_axis',(1.,0.,0.));
#5314=DIRECTION('ref_axis',(0.,0.,-1.));
#5315=DIRECTION('center_axis',(1.,0.,0.));
#5316=DIRECTION('ref_axis',(0.,0.,-1.));
#5317=DIRECTION('center_axis',(1.,0.,0.));
#5318=DIRECTION('ref_axis',(0.,1.,0.));
#5319=DIRECTION('center_axis',(1.,0.,0.));
#5320=DIRECTION('ref_axis',(0.,0.,-1.));
#5321=DIRECTION('',(-1.,0.,0.));
#5322=DIRECTION('center_axis',(-1.,0.,0.));
#5323=DIRECTION('ref_axis',(0.,1.,0.));
#5324=DIRECTION('center_axis',(1.,0.,0.));
#5325=DIRECTION('ref_axis',(0.,0.,-1.));
#5326=DIRECTION('',(-0.832050294337844,-0.554700196225229,-6.79311819793636E-17));
#5327=DIRECTION('center_axis',(1.,0.,0.));
#5328=DIRECTION('ref_axis',(0.,0.,-1.));
#5329=DIRECTION('axis',(0.,0.,1.));
#5330=DIRECTION('refdir',(1.,0.,0.));
#5331=DIRECTION('center_axis',(1.,0.,0.));
#5332=DIRECTION('ref_axis',(0.,1.,0.));
#5333=DIRECTION('center_axis',(1.,0.,0.));
#5334=DIRECTION('ref_axis',(0.,0.,-1.));
#5335=DIRECTION('',(-0.970142500145332,0.242535625036333,2.97020476879948E-17));
#5336=DIRECTION('center_axis',(1.,0.,0.));
#5337=DIRECTION('ref_axis',(0.,0.,-1.));
#5338=DIRECTION('center_axis',(-1.,0.,0.));
#5339=DIRECTION('ref_axis',(0.,0.,1.));
#5340=DIRECTION('center_axis',(1.,0.,0.));
#5341=DIRECTION('ref_axis',(0.,0.,-1.));
#5342=DIRECTION('center_axis',(-1.,0.,0.));
#5343=DIRECTION('ref_axis',(0.,1.,0.));
#5344=DIRECTION('',(-0.970142500145332,-0.242535625036333,-2.97020476879948E-17));
#5345=DIRECTION('center_axis',(1.,0.,0.));
#5346=DIRECTION('ref_axis',(0.,0.,-1.));
#5347=DIRECTION('center_axis',(-1.,0.,0.));
#5348=DIRECTION('ref_axis',(0.,0.,1.));
#5349=DIRECTION('center_axis',(1.,0.,0.));
#5350=DIRECTION('ref_axis',(0.,0.,-1.));
#5351=DIRECTION('center_axis',(1.,0.,0.));
#5352=DIRECTION('ref_axis',(0.,1.,0.));
#5353=DIRECTION('center_axis',(1.,0.,0.));
#5354=DIRECTION('ref_axis',(0.,0.,-1.));
#5355=DIRECTION('',(-0.707106781186547,0.707106781186548,8.65956056235494E-17));
#5356=DIRECTION('center_axis',(1.,0.,0.));
#5357=DIRECTION('ref_axis',(0.,1.,0.));
#5358=DIRECTION('center_axis',(1.,0.,0.));
#5359=DIRECTION('ref_axis',(0.,0.,-1.));
#5360=DIRECTION('',(-1.,0.,0.));
#5361=DIRECTION('center_axis',(-1.,0.,0.));
#5362=DIRECTION('ref_axis',(0.,1.,0.));
#5363=DIRECTION('center_axis',(1.,0.,0.));
#5364=DIRECTION('ref_axis',(0.,0.,-1.));
#5365=DIRECTION('',(-0.707106781186546,-0.707106781186549,-8.65956056235495E-17));
#5366=DIRECTION('center_axis',(1.,0.,0.));
#5367=DIRECTION('ref_axis',(0.,0.,-1.));
#5368=DIRECTION('center_axis',(1.,0.,0.));
#5369=DIRECTION('ref_axis',(0.,0.,-1.));
#5370=DIRECTION('center_axis',(1.,0.,0.));
#5371=DIRECTION('ref_axis',(0.,1.,0.));
#5372=DIRECTION('',(-0.970142500145332,0.242535625036333,2.97020476879948E-17));
#5373=DIRECTION('center_axis',(1.,0.,0.));
#5374=DIRECTION('ref_axis',(0.,0.,-1.));
#5375=DIRECTION('center_axis',(1.,0.,0.));
#5376=DIRECTION('ref_axis',(0.,0.,-1.));
#5377=DIRECTION('center_axis',(1.,0.,0.));
#5378=DIRECTION('ref_axis',(0.,0.,-1.));
#5379=DIRECTION('center_axis',(-1.,0.,0.));
#5380=DIRECTION('ref_axis',(0.,1.,0.));
#5381=DIRECTION('center_axis',(1.,0.,0.));
#5382=DIRECTION('ref_axis',(0.,0.,-1.));
#5383=DIRECTION('',(-0.970142500145332,-0.242535625036333,-2.97020476879948E-17));
#5384=DIRECTION('center_axis',(1.,0.,0.));
#5385=DIRECTION('ref_axis',(0.,0.,-1.));
#5386=DIRECTION('center_axis',(1.,0.,0.));
#5387=DIRECTION('ref_axis',(0.,0.,-1.));
#5388=DIRECTION('center_axis',(1.,0.,0.));
#5389=DIRECTION('ref_axis',(0.,1.,0.));
#5390=DIRECTION('',(-0.707106781186546,0.707106781186549,8.65956056235495E-17));
#5391=DIRECTION('center_axis',(1.,0.,0.));
#5392=DIRECTION('ref_axis',(0.,0.,-1.));
#5393=DIRECTION('center_axis',(1.,0.,0.));
#5394=DIRECTION('ref_axis',(0.,1.,0.));
#5395=DIRECTION('',(-1.,0.,0.));
#5396=DIRECTION('center_axis',(1.,0.,0.));
#5397=DIRECTION('ref_axis',(0.,0.,-1.));
#5398=DIRECTION('center_axis',(-1.,0.,0.));
#5399=DIRECTION('ref_axis',(0.,1.,0.));
#5400=DIRECTION('',(-0.707106781186547,-0.707106781186548,-8.65956056235494E-17));
#5401=DIRECTION('center_axis',(1.,0.,0.));
#5402=DIRECTION('ref_axis',(0.,0.,-1.));
#5403=DIRECTION('center_axis',(-1.,0.,0.));
#5404=DIRECTION('ref_axis',(0.,0.,1.));
#5405=DIRECTION('axis',(0.,0.,1.));
#5406=DIRECTION('refdir',(1.,0.,0.));
#5407=DIRECTION('center_axis',(1.,0.,0.));
#5408=DIRECTION('ref_axis',(0.,1.,0.));
#5409=DIRECTION('center_axis',(1.,0.,0.));
#5410=DIRECTION('ref_axis',(0.,0.,-1.));
#5411=DIRECTION('',(-1.,0.,0.));
#5412=DIRECTION('center_axis',(1.,0.,0.));
#5413=DIRECTION('ref_axis',(0.,0.,-1.));
#5414=DIRECTION('center_axis',(-1.,0.,0.));
#5415=DIRECTION('ref_axis',(0.,0.,1.));
#5416=DIRECTION('center_axis',(1.,0.,0.));
#5417=DIRECTION('ref_axis',(0.,0.,-1.));
#5418=DIRECTION('center_axis',(1.,0.,0.));
#5419=DIRECTION('ref_axis',(0.,1.,0.));
#5420=DIRECTION('center_axis',(1.,0.,0.));
#5421=DIRECTION('ref_axis',(0.,0.,-1.));
#5422=DIRECTION('',(-1.,0.,0.));
#5423=DIRECTION('center_axis',(1.,0.,0.));
#5424=DIRECTION('ref_axis',(0.,0.,-1.));
#5425=DIRECTION('axis',(0.,0.,1.));
#5426=DIRECTION('refdir',(1.,0.,0.));
#5427=DIRECTION('center_axis',(0.,-0.707106781186548,0.707106781186548));
#5428=DIRECTION('ref_axis',(1.,0.,0.));
#5429=DIRECTION('',(1.,0.,0.));
#5430=DIRECTION('',(-1.,0.,0.));
#5431=DIRECTION('center_axis',(0.,-1.,0.));
#5432=DIRECTION('ref_axis',(1.,0.,0.));
#5433=DIRECTION('',(0.,0.,1.));
#5434=DIRECTION('',(-1.,0.,0.));
#5435=DIRECTION('',(0.,0.,1.));
#5436=DIRECTION('center_axis',(0.,-0.707106781186548,0.707106781186548));
#5437=DIRECTION('ref_axis',(1.,0.,0.));
#5438=DIRECTION('',(1.,0.,0.));
#5439=DIRECTION('',(-1.,0.,0.));
#5440=DIRECTION('center_axis',(0.,-1.,0.));
#5441=DIRECTION('ref_axis',(1.,0.,0.));
#5442=DIRECTION('',(0.,0.,1.));
#5443=DIRECTION('',(-1.,0.,0.));
#5444=DIRECTION('',(0.,0.,1.));
#5445=DIRECTION('center_axis',(0.,0.707106781186548,0.707106781186548));
#5446=DIRECTION('ref_axis',(1.,0.,0.));
#5447=DIRECTION('',(-1.,0.,0.));
#5448=DIRECTION('',(1.,0.,0.));
#5449=DIRECTION('center_axis',(0.,1.,0.));
#5450=DIRECTION('ref_axis',(-1.,0.,0.));
#5451=DIRECTION('',(0.,0.,1.));
#5452=DIRECTION('',(1.,0.,0.));
#5453=DIRECTION('',(0.,0.,1.));
#5454=DIRECTION('center_axis',(0.,0.707106781186548,0.707106781186548));
#5455=DIRECTION('ref_axis',(1.,0.,0.));
#5456=DIRECTION('',(-1.,0.,0.));
#5457=DIRECTION('',(1.,0.,0.));
#5458=DIRECTION('center_axis',(0.,1.,0.));
#5459=DIRECTION('ref_axis',(-1.,0.,0.));
#5460=DIRECTION('',(0.,0.,1.));
#5461=DIRECTION('',(1.,0.,0.));
#5462=DIRECTION('',(0.,0.,1.));
#5463=DIRECTION('center_axis',(0.,-0.707106781186548,-0.707106781186548));
#5464=DIRECTION('ref_axis',(-1.,0.,0.));
#5465=DIRECTION('',(1.,0.,0.));
#5466=DIRECTION('center_axis',(0.,0.,1.));
#5467=DIRECTION('ref_axis',(1.,0.,0.));
#5468=DIRECTION('center_axis',(0.,0.,1.));
#5469=DIRECTION('ref_axis',(1.,0.,0.));
#5470=DIRECTION('center_axis',(0.,0.,-1.));
#5471=DIRECTION('ref_axis',(1.,0.,0.));
#5472=DIRECTION('center_axis',(0.,0.,1.));
#5473=DIRECTION('ref_axis',(1.,0.,0.));
#5474=DIRECTION('center_axis',(0.,0.,-1.));
#5475=DIRECTION('ref_axis',(1.,0.,0.));
#5476=DIRECTION('center_axis',(0.,0.,1.));
#5477=DIRECTION('ref_axis',(1.,0.,0.));
#5478=DIRECTION('center_axis',(0.,-0.707106781186548,-0.707106781186548));
#5479=DIRECTION('ref_axis',(-1.,0.,0.));
#5480=DIRECTION('',(1.,0.,0.));
#5481=DIRECTION('center_axis',(0.,0.707106781186548,-0.707106781186548));
#5482=DIRECTION('ref_axis',(-1.,0.,0.));
#5483=DIRECTION('',(-1.,0.,0.));
#5484=DIRECTION('center_axis',(0.,0.,1.));
#5485=DIRECTION('ref_axis',(1.,0.,0.));
#5486=DIRECTION('center_axis',(0.,0.,-1.));
#5487=DIRECTION('ref_axis',(1.,0.,0.));
#5488=DIRECTION('center_axis',(0.,0.,-1.));
#5489=DIRECTION('ref_axis',(1.,0.,0.));
#5490=DIRECTION('center_axis',(0.,0.,1.));
#5491=DIRECTION('ref_axis',(1.,0.,0.));
#5492=DIRECTION('center_axis',(0.,0.707106781186548,-0.707106781186548));
#5493=DIRECTION('ref_axis',(-1.,0.,0.));
#5494=DIRECTION('',(-1.,0.,0.));
#5495=DIRECTION('center_axis',(0.,0.,1.));
#5496=DIRECTION('ref_axis',(-1.,0.,0.));
#5497=DIRECTION('center_axis',(0.,0.,-1.));
#5498=DIRECTION('ref_axis',(-1.,0.,0.));
#5499=DIRECTION('center_axis',(0.,0.,1.));
#5500=DIRECTION('ref_axis',(-1.,0.,0.));
#5501=DIRECTION('center_axis',(0.,0.,1.));
#5502=DIRECTION('ref_axis',(-1.,-3.21624529935327E-16,0.));
#5503=DIRECTION('center_axis',(0.,0.,1.));
#5504=DIRECTION('ref_axis',(-1.,0.,0.));
#5505=DIRECTION('center_axis',(0.,0.,1.));
#5506=DIRECTION('ref_axis',(1.,0.,0.));
#5507=DIRECTION('center_axis',(0.,0.,1.));
#5508=DIRECTION('ref_axis',(1.,0.,0.));
#5509=DIRECTION('center_axis',(0.,0.,1.));
#5510=DIRECTION('ref_axis',(1.,0.,0.));
#5511=DIRECTION('center_axis',(0.,0.,1.));
#5512=DIRECTION('ref_axis',(1.,0.,0.));
#5513=DIRECTION('center_axis',(0.,0.,1.));
#5514=DIRECTION('ref_axis',(1.,0.,0.));
#5515=DIRECTION('center_axis',(0.,0.,1.));
#5516=DIRECTION('ref_axis',(1.,0.,0.));
#5517=DIRECTION('center_axis',(0.,0.,1.));
#5518=DIRECTION('ref_axis',(1.,0.,0.));
#5519=DIRECTION('center_axis',(0.,0.,1.));
#5520=DIRECTION('ref_axis',(1.,0.,0.));
#5521=DIRECTION('center_axis',(0.,0.,1.));
#5522=DIRECTION('ref_axis',(1.,0.,0.));
#5523=DIRECTION('center_axis',(0.,0.,1.));
#5524=DIRECTION('ref_axis',(1.,0.,0.));
#5525=DIRECTION('center_axis',(0.,0.,-1.));
#5526=DIRECTION('ref_axis',(1.,0.,0.));
#5527=DIRECTION('center_axis',(0.,0.,-1.));
#5528=DIRECTION('ref_axis',(1.,0.,0.));
#5529=DIRECTION('center_axis',(0.,0.,-1.));
#5530=DIRECTION('ref_axis',(1.,0.,0.));
#5531=DIRECTION('center_axis',(0.,0.,1.));
#5532=DIRECTION('ref_axis',(1.,0.,0.));
#5533=DIRECTION('center_axis',(0.,0.,-1.));
#5534=DIRECTION('ref_axis',(1.,0.,0.));
#5535=DIRECTION('center_axis',(0.,0.,1.));
#5536=DIRECTION('ref_axis',(1.,0.,0.));
#5537=DIRECTION('center_axis',(0.,-1.,0.));
#5538=DIRECTION('ref_axis',(1.,0.,0.));
#5539=DIRECTION('',(0.,-1.,0.));
#5540=DIRECTION('center_axis',(0.,-1.,0.));
#5541=DIRECTION('ref_axis',(1.,0.,0.));
#5542=DIRECTION('center_axis',(0.,-1.,0.));
#5543=DIRECTION('ref_axis',(1.,0.,0.));
#5544=DIRECTION('center_axis',(0.,-1.,0.));
#5545=DIRECTION('ref_axis',(1.,0.,0.));
#5546=DIRECTION('center_axis',(0.,0.,-1.));
#5547=DIRECTION('ref_axis',(-1.,0.,0.));
#5548=DIRECTION('center_axis',(0.,0.,-1.));
#5549=DIRECTION('ref_axis',(-1.,0.,0.));
#5550=DIRECTION('center_axis',(0.,0.,-1.));
#5551=DIRECTION('ref_axis',(1.,0.,0.));
#5552=DIRECTION('center_axis',(0.,0.,-1.));
#5553=DIRECTION('ref_axis',(1.,0.,0.));
#5554=DIRECTION('center_axis',(0.,0.,1.));
#5555=DIRECTION('ref_axis',(1.,0.,0.));
#5556=DIRECTION('center_axis',(0.,0.,1.));
#5557=DIRECTION('ref_axis',(1.,0.,0.));
#5558=DIRECTION('',(0.707106781186547,8.65956056235492E-17,-0.707106781186548));
#5559=DIRECTION('center_axis',(0.,0.,-1.));
#5560=DIRECTION('ref_axis',(1.,0.,0.));
#5561=DIRECTION('center_axis',(0.,0.,-1.));
#5562=DIRECTION('ref_axis',(1.,0.,0.));
#5563=DIRECTION('center_axis',(0.,0.,1.));
#5564=DIRECTION('ref_axis',(1.,0.,0.));
#5565=DIRECTION('center_axis',(0.,0.,-1.));
#5566=DIRECTION('ref_axis',(1.,0.,0.));
#5567=DIRECTION('center_axis',(0.,0.,-1.));
#5568=DIRECTION('ref_axis',(1.,0.,0.));
#5569=DIRECTION('center_axis',(0.,1.,0.));
#5570=DIRECTION('ref_axis',(1.,0.,0.));
#5571=DIRECTION('',(0.,0.,1.));
#5572=DIRECTION('center_axis',(0.,1.,0.));
#5573=DIRECTION('ref_axis',(1.,0.,0.));
#5574=DIRECTION('',(0.,0.,-1.));
#5575=DIRECTION('center_axis',(0.,0.,-1.));
#5576=DIRECTION('ref_axis',(1.,0.,0.));
#5577=DIRECTION('',(0.,0.,-1.));
#5578=DIRECTION('center_axis',(0.,0.,-1.));
#5579=DIRECTION('ref_axis',(1.,0.,0.));
#5580=DIRECTION('',(0.,0.,-1.));
#5581=DIRECTION('center_axis',(0.,0.,-1.));
#5582=DIRECTION('ref_axis',(1.,0.,0.));
#5583=DIRECTION('',(0.,0.,-1.));
#5584=DIRECTION('axis',(0.,0.,1.));
#5585=DIRECTION('refdir',(1.,0.,0.));
#5586=DIRECTION('center_axis',(1.,0.,0.));
#5587=DIRECTION('ref_axis',(0.,1.,0.));
#5588=DIRECTION('',(-1.,0.,0.));
#5589=DIRECTION('center_axis',(1.,0.,0.));
#5590=DIRECTION('ref_axis',(0.,1.,0.));
#5591=DIRECTION('center_axis',(1.,0.,0.));
#5592=DIRECTION('ref_axis',(0.,1.,0.));
#5593=DIRECTION('',(-1.,0.,0.));
#5594=DIRECTION('center_axis',(1.,0.,0.));
#5595=DIRECTION('ref_axis',(0.,1.,0.));
#5596=DIRECTION('',(-1.,0.,0.));
#5597=DIRECTION('center_axis',(1.,0.,0.));
#5598=DIRECTION('ref_axis',(0.,1.,0.));
#5599=DIRECTION('',(-1.,0.,0.));
#5600=DIRECTION('center_axis',(1.,0.,0.));
#5601=DIRECTION('ref_axis',(0.,1.,0.));
#5602=DIRECTION('',(-1.,0.,0.));
#5603=DIRECTION('center_axis',(1.,0.,0.));
#5604=DIRECTION('ref_axis',(0.,1.,0.));
#5605=DIRECTION('',(-1.,0.,0.));
#5606=DIRECTION('center_axis',(1.,0.,0.));
#5607=DIRECTION('ref_axis',(9.38957226509774E-17,0.703402809462063,-0.710791451581177));
#5608=DIRECTION('',(1.,0.,0.));
#5609=DIRECTION('center_axis',(1.,0.,0.));
#5610=DIRECTION('ref_axis',(9.38957226509774E-17,1.,7.2918327227141E-15));
#5611=DIRECTION('center_axis',(1.,0.,0.));
#5612=DIRECTION('ref_axis',(9.38957226509774E-17,1.,7.2918327227141E-15));
#5613=DIRECTION('',(1.,0.,0.));
#5614=DIRECTION('center_axis',(1.,0.,0.));
#5615=DIRECTION('ref_axis',(9.38957226509774E-17,1.,7.2918327227141E-15));
#5616=DIRECTION('',(1.,0.,0.));
#5617=DIRECTION('center_axis',(1.,0.,0.));
#5618=DIRECTION('ref_axis',(9.38957226509774E-17,1.,7.2918327227141E-15));
#5619=DIRECTION('',(1.,0.,0.));
#5620=DIRECTION('center_axis',(1.,0.,0.));
#5621=DIRECTION('ref_axis',(9.38957226509774E-17,1.,7.2918327227141E-15));
#5622=DIRECTION('',(1.,0.,0.));
#5623=DIRECTION('center_axis',(1.,0.,0.));
#5624=DIRECTION('ref_axis',(0.,0.,-1.));
#5625=DIRECTION('center_axis',(-1.,0.,0.));
#5626=DIRECTION('ref_axis',(0.,1.,0.));
#5627=DIRECTION('center_axis',(-1.,0.,0.));
#5628=DIRECTION('ref_axis',(0.,1.,0.));
#5629=DIRECTION('center_axis',(1.,0.,0.));
#5630=DIRECTION('ref_axis',(0.,0.,-1.));
#5631=DIRECTION('center_axis',(1.,0.,0.));
#5632=DIRECTION('ref_axis',(0.,1.,0.));
#5633=DIRECTION('center_axis',(1.,0.,0.));
#5634=DIRECTION('ref_axis',(0.,1.,0.));
#5635=DIRECTION('center_axis',(-1.,0.,0.));
#5636=DIRECTION('ref_axis',(9.38957226509774E-17,1.,7.2918327227141E-15));
#5637=DIRECTION('center_axis',(1.,0.,0.));
#5638=DIRECTION('ref_axis',(9.38957226509774E-17,1.,7.2918327227141E-15));
#5639=DIRECTION('center_axis',(0.,0.5,-0.866025403784439));
#5640=DIRECTION('ref_axis',(0.,0.866025403784439,0.5));
#5641=DIRECTION('',(0.,0.866025403784439,0.5));
#5642=DIRECTION('',(1.,0.,0.));
#5643=DIRECTION('',(0.,0.866025403784439,0.5));
#5644=DIRECTION('',(1.,0.,0.));
#5645=DIRECTION('center_axis',(0.,-0.5,-0.866025403784439));
#5646=DIRECTION('ref_axis',(0.,0.866025403784439,-0.5));
#5647=DIRECTION('',(0.,0.866025403784439,-0.5));
#5648=DIRECTION('',(1.,0.,0.));
#5649=DIRECTION('',(0.,0.866025403784439,-0.5));
#5650=DIRECTION('center_axis',(0.,-1.,-1.33539075443303E-16));
#5651=DIRECTION('ref_axis',(0.,1.33539075443303E-16,-1.));
#5652=DIRECTION('',(0.,1.33539075443303E-16,-1.));
#5653=DIRECTION('',(1.,0.,0.));
#5654=DIRECTION('',(0.,1.33539075443303E-16,-1.));
#5655=DIRECTION('center_axis',(0.,-0.5,0.866025403784439));
#5656=DIRECTION('ref_axis',(0.,-0.866025403784439,-0.5));
#5657=DIRECTION('',(0.,-0.866025403784439,-0.5));
#5658=DIRECTION('',(1.,0.,0.));
#5659=DIRECTION('',(0.,-0.866025403784439,-0.5));
#5660=DIRECTION('center_axis',(0.,0.5,0.866025403784439));
#5661=DIRECTION('ref_axis',(0.,-0.866025403784439,0.5));
#5662=DIRECTION('',(0.,-0.866025403784439,0.5));
#5663=DIRECTION('',(1.,0.,0.));
#5664=DIRECTION('',(0.,-0.866025403784439,0.5));
#5665=DIRECTION('center_axis',(0.,1.,-2.67078150886606E-16));
#5666=DIRECTION('ref_axis',(0.,2.67078150886606E-16,1.));
#5667=DIRECTION('',(0.,2.67078150886606E-16,1.));
#5668=DIRECTION('',(0.,2.67078150886606E-16,1.));
#5669=DIRECTION('center_axis',(1.,0.,0.));
#5670=DIRECTION('ref_axis',(0.,0.,-1.));
#5671=DIRECTION('center_axis',(-1.,0.,0.));
#5672=DIRECTION('ref_axis',(0.,0.,1.));
#5673=DIRECTION('center_axis',(1.,0.,0.));
#5674=DIRECTION('ref_axis',(0.,0.,-1.));
#5675=DIRECTION('center_axis',(1.,0.,0.));
#5676=DIRECTION('ref_axis',(0.,1.,0.));
#5677=DIRECTION('',(-0.707106781186547,0.707106781186547,8.65956056235493E-17));
#5678=DIRECTION('center_axis',(1.,0.,0.));
#5679=DIRECTION('ref_axis',(0.,-0.766494216754321,-0.642251209171443));
#5680=DIRECTION('center_axis',(-1.,0.,0.));
#5681=DIRECTION('ref_axis',(0.,1.,0.));
#5682=DIRECTION('center_axis',(-1.,0.,0.));
#5683=DIRECTION('ref_axis',(0.,1.,0.));
#5684=DIRECTION('center_axis',(1.,0.,0.));
#5685=DIRECTION('ref_axis',(0.,0.,-1.));
#5686=DIRECTION('',(-0.624695047554424,-0.78086880944303,-9.56288488038411E-17));
#5687=DIRECTION('center_axis',(1.,0.,0.));
#5688=DIRECTION('ref_axis',(0.,0.,-1.));
#5689=DIRECTION('axis',(0.,0.,1.));
#5690=DIRECTION('refdir',(1.,0.,0.));
#5691=DIRECTION('center_axis',(1.,0.,0.));
#5692=DIRECTION('ref_axis',(0.,1.,0.));
#5693=DIRECTION('',(-1.,0.,0.));
#5694=DIRECTION('center_axis',(1.,0.,0.));
#5695=DIRECTION('ref_axis',(0.,1.,0.));
#5696=DIRECTION('center_axis',(1.,0.,0.));
#5697=DIRECTION('ref_axis',(0.,1.,0.));
#5698=DIRECTION('',(-1.,0.,0.));
#5699=DIRECTION('center_axis',(1.,0.,0.));
#5700=DIRECTION('ref_axis',(0.,1.,0.));
#5701=DIRECTION('',(-1.,0.,0.));
#5702=DIRECTION('center_axis',(1.,0.,0.));
#5703=DIRECTION('ref_axis',(0.,1.,0.));
#5704=DIRECTION('',(-1.,0.,0.));
#5705=DIRECTION('center_axis',(1.,0.,0.));
#5706=DIRECTION('ref_axis',(0.,1.,0.));
#5707=DIRECTION('',(-1.,0.,0.));
#5708=DIRECTION('center_axis',(1.,0.,0.));
#5709=DIRECTION('ref_axis',(0.,-0.548549944708551,-0.836117789644644));
#5710=DIRECTION('',(1.,0.,0.));
#5711=DIRECTION('center_axis',(1.,0.,0.));
#5712=DIRECTION('ref_axis',(0.,1.,2.56286223017387E-15));
#5713=DIRECTION('center_axis',(1.,0.,0.));
#5714=DIRECTION('ref_axis',(0.,1.,2.56286223017387E-15));
#5715=DIRECTION('',(1.,0.,0.));
#5716=DIRECTION('center_axis',(1.,0.,0.));
#5717=DIRECTION('ref_axis',(0.,1.,2.56286223017387E-15));
#5718=DIRECTION('',(1.,0.,0.));
#5719=DIRECTION('center_axis',(1.,0.,0.));
#5720=DIRECTION('ref_axis',(0.,1.,2.56286223017387E-15));
#5721=DIRECTION('',(1.,0.,0.));
#5722=DIRECTION('center_axis',(1.,0.,0.));
#5723=DIRECTION('ref_axis',(0.,1.,2.56286223017387E-15));
#5724=DIRECTION('',(1.,0.,0.));
#5725=DIRECTION('center_axis',(1.,0.,0.));
#5726=DIRECTION('ref_axis',(0.,0.,-1.));
#5727=DIRECTION('center_axis',(1.,0.,0.));
#5728=DIRECTION('ref_axis',(0.,1.,0.));
#5729=DIRECTION('center_axis',(1.,0.,0.));
#5730=DIRECTION('ref_axis',(0.,1.,0.));
#5731=DIRECTION('center_axis',(-1.,0.,0.));
#5732=DIRECTION('ref_axis',(0.,1.,2.56286223017387E-15));
#5733=DIRECTION('center_axis',(1.,0.,0.));
#5734=DIRECTION('ref_axis',(0.,0.889057334805044,0.457795866549002));
#5735=DIRECTION('center_axis',(0.,-1.,0.));
#5736=DIRECTION('ref_axis',(0.,0.,-1.));
#5737=DIRECTION('',(1.,0.,0.));
#5738=DIRECTION('',(0.,0.,-1.));
#5739=DIRECTION('',(-1.,0.,0.));
#5740=DIRECTION('',(0.,0.,1.));
#5741=DIRECTION('center_axis',(0.,1.,0.));
#5742=DIRECTION('ref_axis',(0.,0.,1.));
#5743=DIRECTION('',(1.,0.,0.));
#5744=DIRECTION('',(0.,0.,1.));
#5745=DIRECTION('',(-1.,0.,0.));
#5746=DIRECTION('',(0.,0.,-1.));
#5747=DIRECTION('center_axis',(1.,0.,0.));
#5748=DIRECTION('ref_axis',(0.,0.,-1.));
#5749=DIRECTION('center_axis',(1.,0.,0.));
#5750=DIRECTION('ref_axis',(0.,0.,-1.));
#5751=DIRECTION('center_axis',(1.,0.,0.));
#5752=DIRECTION('ref_axis',(0.,0.,-1.));
#5753=DIRECTION('center_axis',(1.,0.,0.));
#5754=DIRECTION('ref_axis',(0.,0.,-1.));
#5755=DIRECTION('center_axis',(1.,0.,0.));
#5756=DIRECTION('ref_axis',(0.,1.,0.));
#5757=DIRECTION('center_axis',(1.,0.,0.));
#5758=DIRECTION('ref_axis',(0.,0.,-1.));
#5759=DIRECTION('center_axis',(0.,-0.5,-0.866025403784439));
#5760=DIRECTION('ref_axis',(0.,-0.866025403784439,0.5));
#5761=DIRECTION('center_axis',(0.,-0.5,-0.866025403784439));
#5762=DIRECTION('ref_axis',(0.,-0.866025403784439,0.5));
#5763=DIRECTION('',(-1.,0.,0.));
#5764=DIRECTION('',(0.,-0.866025403784439,0.5));
#5765=DIRECTION('',(-1.,0.,0.));
#5766=DIRECTION('center_axis',(0.,-1.,-1.60246890531964E-16));
#5767=DIRECTION('ref_axis',(0.,-1.60246890531964E-16,1.));
#5768=DIRECTION('center_axis',(0.,-1.,-1.60246890531964E-16));
#5769=DIRECTION('ref_axis',(0.,-1.60246890531964E-16,1.));
#5770=DIRECTION('',(0.,-1.60246890531964E-16,1.));
#5771=DIRECTION('',(-1.,0.,0.));
#5772=DIRECTION('center_axis',(0.,-0.5,0.866025403784439));
#5773=DIRECTION('ref_axis',(0.,0.866025403784439,0.5));
#5774=DIRECTION('center_axis',(0.,-0.5,0.866025403784439));
#5775=DIRECTION('ref_axis',(0.,0.866025403784439,0.5));
#5776=DIRECTION('',(0.,0.866025403784439,0.5));
#5777=DIRECTION('',(-1.,0.,0.));
#5778=DIRECTION('center_axis',(0.,0.5,0.866025403784439));
#5779=DIRECTION('ref_axis',(0.,0.866025403784439,-0.5));
#5780=DIRECTION('center_axis',(0.,0.5,0.866025403784439));
#5781=DIRECTION('ref_axis',(0.,0.866025403784439,-0.5));
#5782=DIRECTION('',(0.,0.866025403784439,-0.5));
#5783=DIRECTION('',(-1.,0.,0.));
#5784=DIRECTION('center_axis',(0.,0.5,-0.866025403784439));
#5785=DIRECTION('ref_axis',(0.,-0.866025403784439,-0.5));
#5786=DIRECTION('center_axis',(0.,0.5,-0.866025403784439));
#5787=DIRECTION('ref_axis',(0.,-0.866025403784439,-0.5));
#5788=DIRECTION('',(-1.,0.,0.));
#5789=DIRECTION('',(0.,-0.866025403784439,-0.5));
#5790=DIRECTION('center_axis',(0.,1.,-3.20493781063927E-16));
#5791=DIRECTION('ref_axis',(0.,-3.20493781063927E-16,-1.));
#5792=DIRECTION('center_axis',(0.,1.,-3.20493781063927E-16));
#5793=DIRECTION('ref_axis',(0.,-3.20493781063927E-16,-1.));
#5794=DIRECTION('',(0.,-3.20493781063927E-16,-1.));
#5795=DIRECTION('center_axis',(-1.,0.,0.));
#5796=DIRECTION('ref_axis',(0.,0.,1.));
#5797=DIRECTION('center_axis',(0.,0.,1.));
#5798=DIRECTION('ref_axis',(1.,0.,0.));
#5799=DIRECTION('center_axis',(-1.,0.,0.));
#5800=DIRECTION('ref_axis',(0.,1.,0.));
#5801=DIRECTION('center_axis',(-1.,0.,0.));
#5802=DIRECTION('ref_axis',(0.,1.,0.));
#5803=DIRECTION('center_axis',(1.22464679914735E-16,-1.,0.));
#5804=DIRECTION('ref_axis',(-1.,-1.22464679914735E-16,0.));
#5805=DIRECTION('center_axis',(-1.,0.,0.));
#5806=DIRECTION('ref_axis',(0.,1.,0.));
#5807=DIRECTION('center_axis',(1.22464679914735E-16,-1.,0.));
#5808=DIRECTION('ref_axis',(-1.,-1.22464679914735E-16,0.));
#5809=DIRECTION('center_axis',(-1.,0.,0.));
#5810=DIRECTION('ref_axis',(0.,0.,1.));
#5811=DIRECTION('center_axis',(1.,0.,0.));
#5812=DIRECTION('ref_axis',(0.,0.,-1.));
#5813=DIRECTION('center_axis',(1.,0.,0.));
#5814=DIRECTION('ref_axis',(0.,1.,0.));
#5815=DIRECTION('',(-0.707106781186547,0.707106781186548,8.65956056235494E-17));
#5816=DIRECTION('center_axis',(1.,0.,0.));
#5817=DIRECTION('ref_axis',(0.,1.,0.));
#5818=DIRECTION('center_axis',(1.,0.,0.));
#5819=DIRECTION('ref_axis',(0.,1.,0.));
#5820=DIRECTION('center_axis',(-1.,0.,0.));
#5821=DIRECTION('ref_axis',(0.,0.,1.));
#5822=DIRECTION('center_axis',(1.,0.,0.));
#5823=DIRECTION('ref_axis',(0.,0.,-1.));
#5824=DIRECTION('center_axis',(1.,0.,0.));
#5825=DIRECTION('ref_axis',(0.,1.,0.));
#5826=DIRECTION('center_axis',(1.,0.,0.));
#5827=DIRECTION('ref_axis',(0.,1.,0.));
#5828=DIRECTION('',(-1.,0.,0.));
#5829=DIRECTION('axis',(0.,0.,1.));
#5830=DIRECTION('refdir',(1.,0.,0.));
#5831=DIRECTION('center_axis',(-1.,0.,-9.70486199004632E-16));
#5832=DIRECTION('ref_axis',(0.,-1.,-3.31401861020786E-17));
#5833=DIRECTION('center_axis',(-1.,0.,0.));
#5834=DIRECTION('ref_axis',(0.,-1.,0.));
#5835=DIRECTION('',(-0.382683432365091,0.923879532511287,-2.27628838825947E-16));
#5836=DIRECTION('center_axis',(1.,0.,0.));
#5837=DIRECTION('ref_axis',(0.,-1.,-6.12323399573677E-17));
#5838=DIRECTION('center_axis',(1.,0.,0.));
#5839=DIRECTION('ref_axis',(0.,-1.,-6.12323399573677E-17));
#5840=DIRECTION('center_axis',(-1.,0.,0.));
#5841=DIRECTION('ref_axis',(0.,1.,0.));
#5842=DIRECTION('',(-0.707106781186544,-0.707106781186551,-8.65956056235497E-17));
#5843=DIRECTION('center_axis',(1.,0.,0.));
#5844=DIRECTION('ref_axis',(0.,0.,-1.));
#5845=DIRECTION('center_axis',(1.,0.,0.));
#5846=DIRECTION('ref_axis',(0.,0.,-1.));
#5847=DIRECTION('center_axis',(1.,0.,-9.70486199004632E-16));
#5848=DIRECTION('ref_axis',(0.,-1.,-3.31401861020786E-17));
#5849=DIRECTION('center_axis',(-1.,0.,0.));
#5850=DIRECTION('ref_axis',(0.,-1.,-6.12323399573677E-17));
#5851=DIRECTION('center_axis',(-1.,0.,0.));
#5852=DIRECTION('ref_axis',(0.,-1.,-6.12323399573677E-17));
#5853=DIRECTION('',(-0.382683432365091,-0.923879532511287,2.27628838825947E-16));
#5854=DIRECTION('center_axis',(1.,0.,0.));
#5855=DIRECTION('ref_axis',(0.,-1.,0.));
#5856=DIRECTION('center_axis',(-1.,0.,0.));
#5857=DIRECTION('ref_axis',(0.,0.,1.));
#5858=DIRECTION('center_axis',(1.,0.,0.));
#5859=DIRECTION('ref_axis',(0.,1.,0.));
#5860=DIRECTION('center_axis',(1.,0.,0.));
#5861=DIRECTION('ref_axis',(0.,0.,-1.));
#5862=DIRECTION('',(-0.707106781186548,0.707106781186547,8.65956056235493E-17));
#5863=DIRECTION('center_axis',(0.,0.,-1.));
#5864=DIRECTION('ref_axis',(1.,0.,0.));
#5865=DIRECTION('',(0.,0.,-1.));
#5866=DIRECTION('center_axis',(1.,0.,0.));
#5867=DIRECTION('ref_axis',(0.,1.,0.));
#5868=DIRECTION('',(-1.,0.,0.));
#5869=DIRECTION('axis',(0.,0.,1.));
#5870=DIRECTION('refdir',(1.,0.,0.));
#5871=DIRECTION('center_axis',(0.707106781186548,-0.707106781186548,0.));
#5872=DIRECTION('ref_axis',(0.,0.,-1.));
#5873=DIRECTION('',(-0.707106781186547,-0.707106781186547,0.));
#5874=DIRECTION('',(0.,0.,-1.));
#5875=DIRECTION('',(0.707106781186547,0.707106781186547,0.));
#5876=DIRECTION('',(0.,0.,1.));
#5877=DIRECTION('center_axis',(0.,1.,0.));
#5878=DIRECTION('ref_axis',(0.707106781186547,0.,0.707106781186547));
#5879=DIRECTION('center_axis',(0.,-1.,0.));
#5880=DIRECTION('ref_axis',(0.707106781186548,0.,0.707106781186548));
#5881=DIRECTION('',(0.,-0.707106781186547,-0.707106781186547));
#5882=DIRECTION('center_axis',(0.,1.,0.));
#5883=DIRECTION('ref_axis',(0.707106781186547,0.,0.707106781186547));
#5884=DIRECTION('center_axis',(0.,-0.707106781186548,0.707106781186548));
#5885=DIRECTION('ref_axis',(1.,0.,0.));
#5886=DIRECTION('',(-1.,0.,0.));
#5887=DIRECTION('',(0.,-0.707106781186547,-0.707106781186547));
#5888=DIRECTION('',(1.,0.,0.));
#5889=DIRECTION('center_axis',(0.,0.,-1.));
#5890=DIRECTION('ref_axis',(-1.,0.,0.));
#5891=DIRECTION('center_axis',(0.,0.,-1.));
#5892=DIRECTION('ref_axis',(-1.,0.,0.));
#5893=DIRECTION('',(0.,0.707106781186547,-0.707106781186548));
#5894=DIRECTION('center_axis',(0.,0.,1.));
#5895=DIRECTION('ref_axis',(-1.,0.,0.));
#5896=DIRECTION('center_axis',(0.,0.707106781186548,0.707106781186548));
#5897=DIRECTION('ref_axis',(1.,0.,0.));
#5898=DIRECTION('',(1.,0.,0.));
#5899=DIRECTION('',(0.,0.707106781186548,-0.707106781186547));
#5900=DIRECTION('',(-1.,0.,0.));
#5901=DIRECTION('center_axis',(0.,-1.,0.));
#5902=DIRECTION('ref_axis',(0.707106781186547,0.,0.707106781186547));
#5903=DIRECTION('center_axis',(0.,1.,0.));
#5904=DIRECTION('ref_axis',(0.707106781186548,0.,0.707106781186548));
#5905=DIRECTION('',(-0.707106781186547,0.707106781186548,0.));
#5906=DIRECTION('center_axis',(0.,-1.,0.));
#5907=DIRECTION('ref_axis',(0.707106781186547,0.,0.707106781186547));
#5908=DIRECTION('center_axis',(0.707106781186546,0.707106781186549,0.));
#5909=DIRECTION('ref_axis',(0.,0.,-1.));
#5910=DIRECTION('',(-0.707106781186549,0.707106781186546,0.));
#5911=DIRECTION('',(0.,0.,1.));
#5912=DIRECTION('',(0.,0.,-1.));
#5913=DIRECTION('center_axis',(0.,1.,0.));
#5914=DIRECTION('ref_axis',(-0.896854406292881,0.,-0.442325868464691));
#5915=DIRECTION('center_axis',(0.,-1.,0.));
#5916=DIRECTION('ref_axis',(-0.896854406292881,0.,-0.442325868464691));
#5917=DIRECTION('',(-0.430412823330935,0.707106781186551,-0.561021213067998));
#5918=DIRECTION('center_axis',(0.,1.,0.));
#5919=DIRECTION('ref_axis',(-0.896854406292881,0.,-0.442325868464691));
#5920=DIRECTION('center_axis',(0.,-1.,0.));
#5921=DIRECTION('ref_axis',(-1.83697019872103E-16,0.,-1.));
#5922=DIRECTION('',(0.430412823330939,0.707106781186545,-0.561021213068002));
#5923=DIRECTION('center_axis',(0.,-1.,0.));
#5924=DIRECTION('ref_axis',(1.,0.,0.));
#5925=DIRECTION('center_axis',(0.,1.,0.));
#5926=DIRECTION('ref_axis',(1.,0.,0.));
#5927=DIRECTION('center_axis',(0.,1.,0.));
#5928=DIRECTION('ref_axis',(0.896854406292881,0.,-0.442325868464691));
#5929=DIRECTION('center_axis',(0.,-1.,0.));
#5930=DIRECTION('ref_axis',(0.896854406292881,0.,-0.442325868464691));
#5931=DIRECTION('',(0.707106781186547,0.707106781186547,0.));
#5932=DIRECTION('center_axis',(0.,1.,0.));
#5933=DIRECTION('ref_axis',(0.896854406292881,0.,-0.442325868464691));
#5934=DIRECTION('center_axis',(-0.707106781186546,0.707106781186549,0.));
#5935=DIRECTION('ref_axis',(0.,0.,1.));
#5936=DIRECTION('',(0.707106781186548,0.707106781186547,0.));
#5937=DIRECTION('',(0.,0.,-1.));
#5938=DIRECTION('',(0.,0.,1.));
#5939=DIRECTION('center_axis',(0.,1.,0.));
#5940=DIRECTION('ref_axis',(0.707106781186548,0.,0.707106781186548));
#5941=DIRECTION('center_axis',(0.,-1.,0.));
#5942=DIRECTION('ref_axis',(0.707106781186548,0.,0.707106781186548));
#5943=DIRECTION('',(0.,0.707106781186552,0.707106781186543));
#5944=DIRECTION('center_axis',(0.,1.,0.));
#5945=DIRECTION('ref_axis',(0.707106781186547,0.,0.707106781186547));
#5946=DIRECTION('center_axis',(0.,0.707106781186548,-0.707106781186548));
#5947=DIRECTION('ref_axis',(-1.,0.,0.));
#5948=DIRECTION('',(0.,0.707106781186547,0.707106781186547));
#5949=DIRECTION('',(1.,0.,0.));
#5950=DIRECTION('',(-1.,0.,0.));
#5951=DIRECTION('center_axis',(0.,0.,1.));
#5952=DIRECTION('ref_axis',(-1.,0.,0.));
#5953=DIRECTION('',(0.,-0.707106781186547,0.707106781186548));
#5954=DIRECTION('center_axis',(0.,0.,-1.));
#5955=DIRECTION('ref_axis',(-1.,0.,0.));
#5956=DIRECTION('center_axis',(0.,0.,1.));
#5957=DIRECTION('ref_axis',(-1.,0.,0.));
#5958=DIRECTION('center_axis',(0.,-0.707106781186548,-0.707106781186548));
#5959=DIRECTION('ref_axis',(-1.,0.,0.));
#5960=DIRECTION('',(0.,-0.707106781186547,0.707106781186547));
#5961=DIRECTION('',(-1.,0.,0.));
#5962=DIRECTION('',(1.,0.,0.));
#5963=DIRECTION('center_axis',(0.,-1.,0.));
#5964=DIRECTION('ref_axis',(0.707106781186548,0.,0.707106781186548));
#5965=DIRECTION('center_axis',(0.,1.,0.));
#5966=DIRECTION('ref_axis',(0.707106781186548,0.,0.707106781186548));
#5967=DIRECTION('',(0.707106781186547,-0.707106781186547,0.));
#5968=DIRECTION('center_axis',(0.,-1.,0.));
#5969=DIRECTION('ref_axis',(0.707106781186547,0.,0.707106781186547));
#5970=DIRECTION('center_axis',(-0.707106781186548,-0.707106781186548,0.));
#5971=DIRECTION('ref_axis',(0.,0.,1.));
#5972=DIRECTION('',(0.,0.,-1.));
#5973=DIRECTION('',(0.707106781186547,-0.707106781186547,0.));
#5974=DIRECTION('',(0.,0.,1.));
#5975=DIRECTION('center_axis',(0.,-1.,0.));
#5976=DIRECTION('ref_axis',(0.896854406292881,0.,-0.442325868464691));
#5977=DIRECTION('center_axis',(0.,1.,0.));
#5978=DIRECTION('ref_axis',(0.896854406292881,0.,-0.442325868464691));
#5979=DIRECTION('',(0.430412823330944,-0.707106781186546,-0.561021213067997));
#5980=DIRECTION('center_axis',(0.,-1.,0.));
#5981=DIRECTION('ref_axis',(0.896854406292881,0.,-0.442325868464691));
#5982=DIRECTION('center_axis',(0.,1.,0.));
#5983=DIRECTION('ref_axis',(-1.83697019872103E-16,0.,-1.));
#5984=DIRECTION('center_axis',(0.,-1.,0.));
#5985=DIRECTION('ref_axis',(1.,0.,0.));
#5986=DIRECTION('',(-0.430412823330944,-0.707106781186546,-0.561021213067997));
#5987=DIRECTION('center_axis',(0.,1.,0.));
#5988=DIRECTION('ref_axis',(1.,0.,0.));
#5989=DIRECTION('center_axis',(0.,-1.,0.));
#5990=DIRECTION('ref_axis',(-0.896854406292881,0.,-0.442325868464691));
#5991=DIRECTION('center_axis',(0.,1.,0.));
#5992=DIRECTION('ref_axis',(-0.896854406292881,0.,-0.442325868464691));
#5993=DIRECTION('center_axis',(0.,-1.,0.));
#5994=DIRECTION('ref_axis',(-0.896854406292881,0.,-0.442325868464691));
#5995=DIRECTION('center_axis',(0.,0.,1.));
#5996=DIRECTION('ref_axis',(1.,0.,0.));
#5997=DIRECTION('',(0.,-1.,0.));
#5998=DIRECTION('center_axis',(0.,0.,-1.));
#5999=DIRECTION('ref_axis',(1.,0.,0.));
#6000=DIRECTION('center_axis',(0.,1.,0.));
#6001=DIRECTION('ref_axis',(0.896854406292881,0.,-0.442325868464691));
#6002=DIRECTION('',(0.,-1.,0.));
#6003=DIRECTION('',(0.,1.,0.));
#6004=DIRECTION('center_axis',(0.,1.,0.));
#6005=DIRECTION('ref_axis',(5.0532154980743E-16,0.,-1.));
#6006=DIRECTION('',(0.,1.,0.));
#6007=DIRECTION('center_axis',(0.,1.,0.));
#6008=DIRECTION('ref_axis',(0.707106781186548,0.,0.707106781186548));
#6009=DIRECTION('',(0.,1.,0.));
#6010=DIRECTION('center_axis',(0.,1.,0.));
#6011=DIRECTION('ref_axis',(-0.896854406292882,0.,-0.442325868464691));
#6012=DIRECTION('',(0.,-1.,0.));
#6013=DIRECTION('center_axis',(1.,0.,0.));
#6014=DIRECTION('ref_axis',(0.,1.,0.));
#6015=DIRECTION('center_axis',(0.,-1.,0.));
#6016=DIRECTION('ref_axis',(1.,0.,0.));
#6017=DIRECTION('',(0.,0.,1.));
#6018=DIRECTION('center_axis',(0.,1.,0.));
#6019=DIRECTION('ref_axis',(1.,0.,0.));
#6020=DIRECTION('center_axis',(0.,0.,1.));
#6021=DIRECTION('ref_axis',(-1.,1.22464679914735E-16,0.));
#6022=DIRECTION('',(0.,0.,1.));
#6023=DIRECTION('center_axis',(-1.,0.,0.));
#6024=DIRECTION('ref_axis',(0.,0.,1.));
#6025=DIRECTION('',(0.,-1.,0.));
#6026=DIRECTION('center_axis',(0.,-1.,0.));
#6027=DIRECTION('ref_axis',(0.707106781186548,0.,0.707106781186548));
#6028=DIRECTION('',(0.,1.,0.));
#6029=DIRECTION('center_axis',(0.,1.,0.));
#6030=DIRECTION('ref_axis',(1.,0.,0.));
#6031=DIRECTION('',(0.,1.,0.));
#6032=DIRECTION('center_axis',(0.,-1.,0.));
#6033=DIRECTION('ref_axis',(1.,0.,0.));
#6034=DIRECTION('center_axis',(0.,0.,-1.));
#6035=DIRECTION('ref_axis',(1.,0.,0.));
#6036=DIRECTION('',(0.,0.,-1.));
#6037=DIRECTION('center_axis',(0.,0.,1.));
#6038=DIRECTION('ref_axis',(1.,0.,0.));
#6039=DIRECTION('center_axis',(0.,1.,0.));
#6040=DIRECTION('ref_axis',(-1.,0.,0.));
#6041=DIRECTION('center_axis',(0.,0.,1.));
#6042=DIRECTION('ref_axis',(1.,0.,0.));
#6043=DIRECTION('axis',(0.,0.,1.));
#6044=DIRECTION('refdir',(1.,0.,0.));
#6045=DIRECTION('center_axis',(1.,0.,0.));
#6046=DIRECTION('ref_axis',(0.,1.,0.));
#6047=DIRECTION('center_axis',(1.,0.,0.));
#6048=DIRECTION('ref_axis',(0.,0.,-1.));
#6049=DIRECTION('',(-1.,0.,0.));
#6050=DIRECTION('center_axis',(1.,0.,0.));
#6051=DIRECTION('ref_axis',(0.,0.,-1.));
#6052=DIRECTION('center_axis',(-1.,0.,0.));
#6053=DIRECTION('ref_axis',(0.,0.,1.));
#6054=DIRECTION('center_axis',(1.,0.,0.));
#6055=DIRECTION('ref_axis',(0.,0.,-1.));
#6056=DIRECTION('center_axis',(1.,0.,0.));
#6057=DIRECTION('ref_axis',(0.,1.,0.));
#6058=DIRECTION('center_axis',(1.,0.,0.));
#6059=DIRECTION('ref_axis',(0.,0.,-1.));
#6060=DIRECTION('',(-1.,0.,0.));
#6061=DIRECTION('center_axis',(-1.,0.,0.));
#6062=DIRECTION('ref_axis',(0.,0.,1.));
#6063=DIRECTION('center_axis',(1.,0.,0.));
#6064=DIRECTION('ref_axis',(0.,0.,-1.));
#6065=DIRECTION('center_axis',(1.,0.,0.));
#6066=DIRECTION('ref_axis',(0.,1.,0.));
#6067=DIRECTION('center_axis',(1.,0.,0.));
#6068=DIRECTION('ref_axis',(0.,0.,-1.));
#6069=DIRECTION('',(-1.,0.,0.));
#6070=DIRECTION('center_axis',(1.,0.,0.));
#6071=DIRECTION('ref_axis',(0.,0.,-1.));
#6072=DIRECTION('axis',(0.,0.,1.));
#6073=DIRECTION('refdir',(1.,0.,0.));
#6074=DIRECTION('center_axis',(1.,0.,0.));
#6075=DIRECTION('ref_axis',(0.,1.,0.));
#6076=DIRECTION('',(-1.,0.,0.));
#6077=DIRECTION('center_axis',(1.,0.,0.));
#6078=DIRECTION('ref_axis',(0.,1.,0.));
#6079=DIRECTION('center_axis',(1.,0.,0.));
#6080=DIRECTION('ref_axis',(0.,1.,0.));
#6081=DIRECTION('',(-1.,0.,0.));
#6082=DIRECTION('center_axis',(1.,0.,0.));
#6083=DIRECTION('ref_axis',(0.,1.,0.));
#6084=DIRECTION('',(-1.,0.,0.));
#6085=DIRECTION('center_axis',(1.,0.,0.));
#6086=DIRECTION('ref_axis',(0.,1.,0.));
#6087=DIRECTION('',(-1.,0.,0.));
#6088=DIRECTION('center_axis',(1.,0.,0.));
#6089=DIRECTION('ref_axis',(0.,1.,0.));
#6090=DIRECTION('',(-1.,0.,0.));
#6091=DIRECTION('center_axis',(1.,0.,0.));
#6092=DIRECTION('ref_axis',(0.,1.,0.));
#6093=DIRECTION('',(-1.,0.,0.));
#6094=DIRECTION('center_axis',(1.,0.,0.));
#6095=DIRECTION('ref_axis',(0.,1.,0.));
#6096=DIRECTION('',(-1.,0.,0.));
#6097=DIRECTION('center_axis',(1.,0.,0.));
#6098=DIRECTION('ref_axis',(0.,1.,0.));
#6099=DIRECTION('',(-1.,0.,0.));
#6100=DIRECTION('center_axis',(1.,0.,0.));
#6101=DIRECTION('ref_axis',(0.,1.,0.));
#6102=DIRECTION('',(-1.,0.,0.));
#6103=DIRECTION('center_axis',(1.,0.,0.));
#6104=DIRECTION('ref_axis',(0.,1.,0.));
#6105=DIRECTION('',(-1.,0.,0.));
#6106=DIRECTION('center_axis',(1.,0.,0.));
#6107=DIRECTION('ref_axis',(0.,1.,0.));
#6108=DIRECTION('',(-1.,0.,0.));
#6109=DIRECTION('center_axis',(1.,0.,0.));
#6110=DIRECTION('ref_axis',(0.,1.,0.));
#6111=DIRECTION('',(-1.,0.,0.));
#6112=DIRECTION('center_axis',(1.,0.,0.));
#6113=DIRECTION('ref_axis',(0.,-0.212506567199799,-0.977159638389223));
#6114=DIRECTION('',(1.,0.,0.));
#6115=DIRECTION('center_axis',(1.,0.,0.));
#6116=DIRECTION('ref_axis',(0.,1.,8.16536394665384E-14));
#6117=DIRECTION('center_axis',(1.,0.,0.));
#6118=DIRECTION('ref_axis',(0.,1.,8.16536394665384E-14));
#6119=DIRECTION('',(1.,0.,0.));
#6120=DIRECTION('center_axis',(1.,0.,0.));
#6121=DIRECTION('ref_axis',(0.,1.,8.16536394665384E-14));
#6122=DIRECTION('',(1.,0.,0.));
#6123=DIRECTION('center_axis',(1.,0.,0.));
#6124=DIRECTION('ref_axis',(0.,1.,8.16536394665384E-14));
#6125=DIRECTION('',(1.,0.,0.));
#6126=DIRECTION('center_axis',(1.,0.,0.));
#6127=DIRECTION('ref_axis',(0.,1.,8.16536394665384E-14));
#6128=DIRECTION('',(1.,0.,0.));
#6129=DIRECTION('center_axis',(1.,0.,0.));
#6130=DIRECTION('ref_axis',(0.,1.,8.16536394665384E-14));
#6131=DIRECTION('',(1.,0.,0.));
#6132=DIRECTION('center_axis',(1.,0.,0.));
#6133=DIRECTION('ref_axis',(0.,1.,8.16536394665384E-14));
#6134=DIRECTION('',(1.,0.,0.));
#6135=DIRECTION('center_axis',(1.,0.,0.));
#6136=DIRECTION('ref_axis',(0.,1.,8.16536394665384E-14));
#6137=DIRECTION('',(1.,0.,0.));
#6138=DIRECTION('center_axis',(1.,0.,0.));
#6139=DIRECTION('ref_axis',(0.,1.,8.16536394665384E-14));
#6140=DIRECTION('',(1.,0.,0.));
#6141=DIRECTION('center_axis',(1.,0.,0.));
#6142=DIRECTION('ref_axis',(0.,1.,8.16536394665384E-14));
#6143=DIRECTION('',(1.,0.,0.));
#6144=DIRECTION('center_axis',(1.,0.,0.));
#6145=DIRECTION('ref_axis',(0.,1.,8.16536394665384E-14));
#6146=DIRECTION('',(1.,0.,0.));
#6147=DIRECTION('center_axis',(1.,0.,0.));
#6148=DIRECTION('ref_axis',(0.,1.,8.16536394665384E-14));
#6149=DIRECTION('',(1.,0.,0.));
#6150=DIRECTION('center_axis',(1.,0.,0.));
#6151=DIRECTION('ref_axis',(0.,0.,-1.));
#6152=DIRECTION('center_axis',(1.,0.,0.));
#6153=DIRECTION('ref_axis',(0.,1.,0.));
#6154=DIRECTION('center_axis',(1.,0.,0.));
#6155=DIRECTION('ref_axis',(0.,1.,0.));
#6156=DIRECTION('center_axis',(-1.,0.,0.));
#6157=DIRECTION('ref_axis',(0.,1.,8.16536394665384E-14));
#6158=DIRECTION('center_axis',(1.,0.,0.));
#6159=DIRECTION('ref_axis',(0.,1.,8.16536394665384E-14));
#6160=DIRECTION('center_axis',(0.,-1.,4.73106402539129E-17));
#6161=DIRECTION('ref_axis',(0.,4.73106402539129E-17,1.));
#6162=DIRECTION('',(-1.,0.,0.));
#6163=DIRECTION('',(0.,4.73106402539129E-17,1.));
#6164=DIRECTION('',(-1.,0.,0.));
#6165=DIRECTION('',(0.,4.73106402539129E-17,1.));
#6166=DIRECTION('center_axis',(0.,1.,-4.73106402539129E-17));
#6167=DIRECTION('ref_axis',(0.,-4.73106402539129E-17,-1.));
#6168=DIRECTION('',(1.,0.,0.));
#6169=DIRECTION('',(0.,-4.73106402539129E-17,-1.));
#6170=DIRECTION('',(-1.,0.,0.));
#6171=DIRECTION('',(0.,-4.73106402539129E-17,-1.));
#6172=DIRECTION('center_axis',(0.,1.,-4.73106402539129E-17));
#6173=DIRECTION('ref_axis',(0.,-4.73106402539129E-17,-1.));
#6174=DIRECTION('',(-1.,0.,0.));
#6175=DIRECTION('',(0.,-4.73106402539129E-17,-1.));
#6176=DIRECTION('',(-1.,0.,0.));
#6177=DIRECTION('',(0.,-4.73106402539129E-17,-1.));
#6178=DIRECTION('center_axis',(0.,0.,1.));
#6179=DIRECTION('ref_axis',(0.,1.,0.));
#6180=DIRECTION('',(0.,1.,0.));
#6181=DIRECTION('',(-1.,0.,0.));
#6182=DIRECTION('',(0.,1.,0.));
#6183=DIRECTION('center_axis',(0.,-1.,4.73106402539129E-17));
#6184=DIRECTION('ref_axis',(0.,4.73106402539129E-17,1.));
#6185=DIRECTION('',(1.,0.,0.));
#6186=DIRECTION('',(0.,4.73106402539129E-17,1.));
#6187=DIRECTION('',(0.,4.73106402539129E-17,1.));
#6188=DIRECTION('center_axis',(0.,0.,-1.));
#6189=DIRECTION('ref_axis',(0.,-1.,0.));
#6190=DIRECTION('',(0.,-1.,0.));
#6191=DIRECTION('',(0.,-1.,0.));
#6192=DIRECTION('center_axis',(0.,0.,1.));
#6193=DIRECTION('ref_axis',(0.,1.,0.));
#6194=DIRECTION('',(0.,1.,0.));
#6195=DIRECTION('',(-1.,0.,0.));
#6196=DIRECTION('',(0.,1.,0.));
#6197=DIRECTION('center_axis',(1.,0.,0.));
#6198=DIRECTION('ref_axis',(0.,0.,-1.));
#6199=DIRECTION('center_axis',(1.,0.,0.));
#6200=DIRECTION('ref_axis',(0.,0.,-1.));
#6201=DIRECTION('',(0.,0.,-1.));
#6202=DIRECTION('',(0.,-1.,0.));
#6203=DIRECTION('',(0.,-1.,0.));
#6204=DIRECTION('',(0.,0.,1.));
#6205=DIRECTION('',(0.,1.,0.));
#6206=DIRECTION('center_axis',(0.,0.,-1.));
#6207=DIRECTION('ref_axis',(0.,-1.,0.));
#6208=DIRECTION('',(-1.,0.,0.));
#6209=DIRECTION('',(0.,-1.,0.));
#6210=DIRECTION('center_axis',(0.,1.,0.));
#6211=DIRECTION('ref_axis',(0.,0.,-1.));
#6212=DIRECTION('',(0.,0.,-1.));
#6213=DIRECTION('center_axis',(0.,0.,1.));
#6214=DIRECTION('ref_axis',(0.,1.,0.));
#6215=DIRECTION('',(-1.,0.,0.));
#6216=DIRECTION('',(0.,1.,0.));
#6217=DIRECTION('center_axis',(0.,-1.,0.));
#6218=DIRECTION('ref_axis',(0.,0.,1.));
#6219=DIRECTION('',(-1.,0.,0.));
#6220=DIRECTION('',(0.,0.,1.));
#6221=DIRECTION('center_axis',(0.,0.,-1.));
#6222=DIRECTION('ref_axis',(0.,-1.,0.));
#6223=DIRECTION('',(0.,-1.,0.));
#6224=DIRECTION('center_axis',(-1.,0.,0.));
#6225=DIRECTION('ref_axis',(0.,0.,1.));
#6226=DIRECTION('center_axis',(-1.,0.,0.));
#6227=DIRECTION('ref_axis',(0.,0.,1.));
#6228=DIRECTION('center_axis',(1.,0.,0.));
#6229=DIRECTION('ref_axis',(0.,0.,-1.));
#6230=DIRECTION('center_axis',(1.,0.,0.));
#6231=DIRECTION('ref_axis',(0.,1.,0.));
#6232=DIRECTION('',(-0.707106781186548,0.707106781186547,8.65956056235493E-17));
#6233=DIRECTION('center_axis',(1.,0.,0.));
#6234=DIRECTION('ref_axis',(0.,0.956248839876859,-0.292554535487252));
#6235=DIRECTION('center_axis',(1.,0.,0.));
#6236=DIRECTION('ref_axis',(0.,1.,0.));
#6237=DIRECTION('center_axis',(-1.,0.,0.));
#6238=DIRECTION('ref_axis',(0.,0.,1.));
#6239=DIRECTION('center_axis',(1.,0.,0.));
#6240=DIRECTION('ref_axis',(0.,0.,-1.));
#6241=DIRECTION('center_axis',(1.,0.,0.));
#6242=DIRECTION('ref_axis',(0.,1.,0.));
#6243=DIRECTION('center_axis',(1.,0.,0.));
#6244=DIRECTION('ref_axis',(0.,0.,-1.));
#6245=DIRECTION('',(-1.,0.,0.));
#6246=DIRECTION('center_axis',(-1.,0.,0.));
#6247=DIRECTION('ref_axis',(0.,1.,0.));
#6248=DIRECTION('',(-0.78086880944303,-0.624695047554425,-7.65030790430729E-17));
#6249=DIRECTION('axis',(0.,0.,1.));
#6250=DIRECTION('refdir',(1.,0.,0.));
#6251=DIRECTION('center_axis',(-1.,0.,0.));
#6252=DIRECTION('ref_axis',(0.,-1.,0.));
#6253=DIRECTION('center_axis',(-1.,0.,0.));
#6254=DIRECTION('ref_axis',(0.,-1.,0.));
#6255=DIRECTION('',(0.707106781186548,-0.707106781186548,8.65956056235493E-17));
#6256=DIRECTION('center_axis',(1.,0.,0.));
#6257=DIRECTION('ref_axis',(0.,-1.,0.));
#6258=DIRECTION('center_axis',(1.,0.,0.));
#6259=DIRECTION('ref_axis',(0.,-1.,0.));
#6260=DIRECTION('center_axis',(1.,0.,0.));
#6261=DIRECTION('ref_axis',(0.,1.,0.));
#6262=DIRECTION('center_axis',(-1.,0.,0.));
#6263=DIRECTION('ref_axis',(0.,-1.,0.));
#6264=DIRECTION('center_axis',(-1.,0.,0.));
#6265=DIRECTION('ref_axis',(0.,-1.,0.));
#6266=DIRECTION('',(-1.,0.,0.));
#6267=DIRECTION('center_axis',(-1.,0.,0.));
#6268=DIRECTION('ref_axis',(0.,0.,1.));
#6269=DIRECTION('center_axis',(1.,0.,0.));
#6270=DIRECTION('ref_axis',(0.,0.,-1.));
#6271=DIRECTION('center_axis',(1.,0.,0.));
#6272=DIRECTION('ref_axis',(0.,-1.,0.));
#6273=DIRECTION('',(0.707106781186548,0.707106781186548,-8.65956056235493E-17));
#6274=DIRECTION('center_axis',(1.,0.,0.));
#6275=DIRECTION('ref_axis',(0.,-1.,0.));
#6276=DIRECTION('center_axis',(1.,0.,0.));
#6277=DIRECTION('ref_axis',(0.,0.,-1.));
#6278=DIRECTION('center_axis',(1.,0.,0.));
#6279=DIRECTION('ref_axis',(0.,0.,-1.));
#6280=DIRECTION('center_axis',(1.,0.,0.));
#6281=DIRECTION('ref_axis',(0.,1.,0.));
#6282=DIRECTION('center_axis',(1.,0.,0.));
#6283=DIRECTION('ref_axis',(0.,0.,-1.));
#6284=DIRECTION('',(-0.707106781186547,0.707106781186548,8.65956056235494E-17));
#6285=DIRECTION('center_axis',(1.,0.,0.));
#6286=DIRECTION('ref_axis',(0.,1.,0.));
#6287=DIRECTION('center_axis',(1.,0.,0.));
#6288=DIRECTION('ref_axis',(0.,0.,-1.));
#6289=DIRECTION('',(-1.,0.,0.));
#6290=DIRECTION('center_axis',(-1.,0.,0.));
#6291=DIRECTION('ref_axis',(0.,1.,0.));
#6292=DIRECTION('',(-0.707106781186547,-0.707106781186547,-8.65956056235493E-17));
#6293=DIRECTION('',(0.,0.,1.));
#6294=DIRECTION('',(1.,0.,0.));
#6295=DIRECTION('',(0.,1.,0.));
#6296=DIRECTION('',(0.,0.,1.));
#6297=DIRECTION('',(0.,1.,0.));
#6298=DIRECTION('',(0.,0.,1.));
#6299=DIRECTION('',(0.,1.,0.));
#6300=DIRECTION('',(0.,0.,1.));
#6301=DIRECTION('',(0.,1.,0.));
#6302=DIRECTION('',(0.,0.,1.));
#6303=DIRECTION('',(0.,0.,1.));
#6304=DIRECTION('',(1.,0.,0.));
#6305=DIRECTION('',(0.,0.,1.));
#6306=DIRECTION('',(0.,-1.,0.));
#6307=DIRECTION('',(0.,0.,1.));
#6308=DIRECTION('',(0.,-1.,0.));
#6309=DIRECTION('',(0.,1.,0.));
#6310=DIRECTION('',(0.,0.,1.));
#6311=DIRECTION('',(0.,0.,1.));
#6312=DIRECTION('',(-1.,-3.33066907387547E-16,0.));
#6313=DIRECTION('',(0.,1.,0.));
#6314=DIRECTION('',(0.,0.,1.));
#6315=DIRECTION('',(0.,1.,0.));
#6316=DIRECTION('',(0.,0.,1.));
#6317=DIRECTION('',(0.,0.,-1.));
#6318=DIRECTION('',(-3.33066907387547E-16,1.,0.));
#6319=DIRECTION('',(0.,0.,1.));
#6320=DIRECTION('',(1.,3.33066907387547E-16,0.));
#6321=DIRECTION('',(0.,1.,0.));
#6322=DIRECTION('',(0.,0.,1.));
#6323=DIRECTION('',(0.,1.,0.));
#6324=DIRECTION('',(0.,0.,1.));
#6325=DIRECTION('',(0.,0.,-1.));
#6326=DIRECTION('',(-3.33066907387547E-16,1.,0.));
#6327=CARTESIAN_POINT('',(0.,0.,0.));
#6328=CARTESIAN_POINT('',(0.,0.,0.));
#6329=CARTESIAN_POINT('Origin',(0.,-8.02,4.));
#6330=CARTESIAN_POINT('',(-2.64,-8.2,4.));
#6331=CARTESIAN_POINT('Origin',(0.,-8.2,4.));
#6332=CARTESIAN_POINT('',(-3.,-7.84,4.));
#6333=CARTESIAN_POINT('',(-2.82,-8.02,4.));
#6334=CARTESIAN_POINT('Origin',(0.,-7.84,4.));
#6335=CARTESIAN_POINT('Origin',(0.,-7.,4.));
#6336=CARTESIAN_POINT('',(-3.,-7.,4.));
#6337=CARTESIAN_POINT('',(-3.,-7.,4.));
#6338=CARTESIAN_POINT('',(3.,-7.,4.));
#6339=CARTESIAN_POINT('Origin',(0.,-7.,4.));
#6340=CARTESIAN_POINT('Origin',(0.,-7.,4.));
#6341=CARTESIAN_POINT('Origin',(0.,-8.2,4.));
#6342=CARTESIAN_POINT('',(-1.3,-8.2,4.));
#6343=CARTESIAN_POINT('Origin',(0.,-8.2,4.));
#6344=CARTESIAN_POINT('Origin',(0.,0.,8.9));
#6345=CARTESIAN_POINT('',(-5.205,-6.37428658956197E-16,9.));
#6346=CARTESIAN_POINT('Origin',(0.,0.,9.));
#6347=CARTESIAN_POINT('',(-5.005,6.1293572297325E-16,8.8));
#6348=CARTESIAN_POINT('',(-5.105,-6.25182190964724E-16,8.9));
#6349=CARTESIAN_POINT('Origin',(0.,0.,8.8));
#6350=CARTESIAN_POINT('Origin',(0.,0.,9.));
#6351=CARTESIAN_POINT('',(3.,-6.6,9.));
#6352=CARTESIAN_POINT('',(-3.,-6.6,9.));
#6353=CARTESIAN_POINT('',(-1.5,-6.6,9.));
#6354=CARTESIAN_POINT('',(6.6,-3.,9.));
#6355=CARTESIAN_POINT('Origin',(3.,-3.,9.));
#6356=CARTESIAN_POINT('',(6.6,3.,9.));
#6357=CARTESIAN_POINT('',(6.6,-1.5,9.));
#6358=CARTESIAN_POINT('',(3.,6.6,9.));
#6359=CARTESIAN_POINT('Origin',(3.,3.,9.));
#6360=CARTESIAN_POINT('',(-3.,6.6,9.));
#6361=CARTESIAN_POINT('',(1.5,6.6,9.));
#6362=CARTESIAN_POINT('',(-6.6,3.,9.));
#6363=CARTESIAN_POINT('Origin',(-3.,3.,9.));
#6364=CARTESIAN_POINT('',(-6.6,-3.,9.));
#6365=CARTESIAN_POINT('',(-6.6,1.5,9.));
#6366=CARTESIAN_POINT('Origin',(-3.,-3.,9.));
#6367=CARTESIAN_POINT('Origin',(0.,0.,7.55));
#6368=CARTESIAN_POINT('',(-5.005,-6.1293572297325E-16,6.));
#6369=CARTESIAN_POINT('Origin',(0.,0.,6.));
#6370=CARTESIAN_POINT('',(-5.005,-6.1293572297325E-16,7.55));
#6371=CARTESIAN_POINT('Origin',(0.,0.,0.1));
#6372=CARTESIAN_POINT('',(-5.205,6.37428658956197E-16,0.));
#6373=CARTESIAN_POINT('Origin',(0.,0.,0.));
#6374=CARTESIAN_POINT('',(-5.005,-6.1293572297325E-16,0.2));
#6375=CARTESIAN_POINT('',(-5.105,6.25182190964724E-16,0.1));
#6376=CARTESIAN_POINT('Origin',(0.,0.,0.2));
#6377=CARTESIAN_POINT('Origin',(0.,0.,0.));
#6378=CARTESIAN_POINT('',(-3.,-6.6,0.));
#6379=CARTESIAN_POINT('',(3.,-6.6,0.));
#6380=CARTESIAN_POINT('',(-1.5,-6.6,0.));
#6381=CARTESIAN_POINT('',(-6.6,-3.,0.));
#6382=CARTESIAN_POINT('Origin',(-3.,-3.,0.));
#6383=CARTESIAN_POINT('',(-6.6,3.,0.));
#6384=CARTESIAN_POINT('',(-6.6,1.5,0.));
#6385=CARTESIAN_POINT('',(-3.,6.6,0.));
#6386=CARTESIAN_POINT('Origin',(-3.,3.,0.));
#6387=CARTESIAN_POINT('',(3.,6.6,0.));
#6388=CARTESIAN_POINT('',(1.5,6.6,0.));
#6389=CARTESIAN_POINT('',(6.6,3.,0.));
#6390=CARTESIAN_POINT('Origin',(3.,3.,0.));
#6391=CARTESIAN_POINT('',(6.6,-3.,0.));
#6392=CARTESIAN_POINT('',(6.6,-1.5,0.));
#6393=CARTESIAN_POINT('Origin',(3.,-3.,0.));
#6394=CARTESIAN_POINT('Origin',(0.,0.,1.45));
#6395=CARTESIAN_POINT('',(-5.005,-6.1293572297325E-16,3.));
#6396=CARTESIAN_POINT('',(-5.005,-6.1293572297325E-16,1.45));
#6397=CARTESIAN_POINT('Origin',(0.,0.,3.));
#6398=CARTESIAN_POINT('Origin',(-1.5,-6.8,0.2));
#6399=CARTESIAN_POINT('',(3.,-7.,0.4));
#6400=CARTESIAN_POINT('',(3.,-6.6,0.));
#6401=CARTESIAN_POINT('',(-3.,-7.,0.4));
#6402=CARTESIAN_POINT('',(-1.5,-7.,0.4));
#6403=CARTESIAN_POINT('',(-3.,-7.,0.4));
#6404=CARTESIAN_POINT('Origin',(3.,-3.,0.2));
#6405=CARTESIAN_POINT('',(7.,-3.,0.4));
#6406=CARTESIAN_POINT('',(6.6,-3.,0.));
#6407=CARTESIAN_POINT('Origin',(3.,-3.,0.4));
#6408=CARTESIAN_POINT('Origin',(6.8,-1.5,0.2));
#6409=CARTESIAN_POINT('',(7.,3.,0.4));
#6410=CARTESIAN_POINT('',(6.6,3.,0.));
#6411=CARTESIAN_POINT('',(7.,-1.5,0.4));
#6412=CARTESIAN_POINT('Origin',(3.,3.,0.2));
#6413=CARTESIAN_POINT('',(3.,7.,0.4));
#6414=CARTESIAN_POINT('',(3.,6.6,0.));
#6415=CARTESIAN_POINT('Origin',(3.,3.,0.4));
#6416=CARTESIAN_POINT('Origin',(1.5,6.8,0.2));
#6417=CARTESIAN_POINT('',(-3.,7.,0.4));
#6418=CARTESIAN_POINT('',(-3.,6.6,0.));
#6419=CARTESIAN_POINT('',(1.5,7.,0.4));
#6420=CARTESIAN_POINT('Origin',(-3.,3.,0.2));
#6421=CARTESIAN_POINT('',(-7.,3.,0.4));
#6422=CARTESIAN_POINT('',(-6.6,3.,0.));
#6423=CARTESIAN_POINT('Origin',(-3.,3.,0.4));
#6424=CARTESIAN_POINT('Origin',(-6.8,1.5,0.2));
#6425=CARTESIAN_POINT('',(-7.,-3.,0.4));
#6426=CARTESIAN_POINT('',(-6.6,-3.,0.));
#6427=CARTESIAN_POINT('',(-7.,1.5,0.4));
#6428=CARTESIAN_POINT('Origin',(-3.,-3.,0.2));
#6429=CARTESIAN_POINT('Origin',(-3.,-3.,0.4));
#6430=CARTESIAN_POINT('Origin',(-3.,3.,0.));
#6431=CARTESIAN_POINT('',(-7.,3.,8.6));
#6432=CARTESIAN_POINT('',(-7.,3.,0.));
#6433=CARTESIAN_POINT('',(-3.,7.,8.6));
#6434=CARTESIAN_POINT('Origin',(-3.,3.,8.6));
#6435=CARTESIAN_POINT('',(-3.,7.,0.));
#6436=CARTESIAN_POINT('Origin',(-7.,3.,0.));
#6437=CARTESIAN_POINT('',(-7.,-3.,8.6));
#6438=CARTESIAN_POINT('',(-7.,-3.,0.));
#6439=CARTESIAN_POINT('',(-7.,1.5,8.6));
#6440=CARTESIAN_POINT('Origin',(-3.,-3.,0.));
#6441=CARTESIAN_POINT('',(-3.,-7.,0.));
#6442=CARTESIAN_POINT('',(-3.,-7.,8.6));
#6443=CARTESIAN_POINT('',(-3.,-7.,0.));
#6444=CARTESIAN_POINT('Origin',(-3.,-3.,8.6));
#6445=CARTESIAN_POINT('Origin',(-3.,-7.,0.));
#6446=CARTESIAN_POINT('',(3.,-7.,0.));
#6447=CARTESIAN_POINT('Origin',(-1.5,-6.8,8.8));
#6448=CARTESIAN_POINT('',(3.,-7.,8.6));
#6449=CARTESIAN_POINT('',(3.,-7.,8.6));
#6450=CARTESIAN_POINT('',(-3.,-6.6,9.));
#6451=CARTESIAN_POINT('',(-1.5,-7.,8.6));
#6452=CARTESIAN_POINT('Origin',(3.,-3.,8.8));
#6453=CARTESIAN_POINT('',(7.,-3.,8.6));
#6454=CARTESIAN_POINT('',(7.,-3.,8.6));
#6455=CARTESIAN_POINT('Origin',(3.,-3.,8.6));
#6456=CARTESIAN_POINT('Origin',(6.8,-1.5,8.8));
#6457=CARTESIAN_POINT('',(7.,3.,8.6));
#6458=CARTESIAN_POINT('',(7.,3.,8.6));
#6459=CARTESIAN_POINT('',(7.,-1.5,8.6));
#6460=CARTESIAN_POINT('Origin',(3.,3.,8.8));
#6461=CARTESIAN_POINT('',(3.,7.,8.6));
#6462=CARTESIAN_POINT('',(3.,7.,8.6));
#6463=CARTESIAN_POINT('Origin',(3.,3.,8.6));
#6464=CARTESIAN_POINT('Origin',(1.5,6.8,8.8));
#6465=CARTESIAN_POINT('',(-3.,7.,8.6));
#6466=CARTESIAN_POINT('',(1.5,7.,8.6));
#6467=CARTESIAN_POINT('Origin',(-3.,3.,8.8));
#6468=CARTESIAN_POINT('',(-7.,3.,8.6));
#6469=CARTESIAN_POINT('Origin',(-6.8,1.5,8.8));
#6470=CARTESIAN_POINT('',(-7.,-3.,8.6));
#6471=CARTESIAN_POINT('Origin',(-3.,-3.,8.8));
#6472=CARTESIAN_POINT('Origin',(3.,3.,0.));
#6473=CARTESIAN_POINT('',(3.,7.,0.));
#6474=CARTESIAN_POINT('',(7.,3.,0.));
#6475=CARTESIAN_POINT('Origin',(7.,-3.,0.));
#6476=CARTESIAN_POINT('',(7.,-3.,0.));
#6477=CARTESIAN_POINT('Origin',(3.,-3.,0.));
#6478=CARTESIAN_POINT('',(3.,-7.,0.));
#6479=CARTESIAN_POINT('Origin',(-3.,-7.,0.));
#6480=CARTESIAN_POINT('Origin',(0.,-8.2,4.));
#6481=CARTESIAN_POINT('',(-1.3,-5.6,4.));
#6482=CARTESIAN_POINT('',(-1.3,-8.2,4.));
#6483=CARTESIAN_POINT('Origin',(0.,-5.6,4.));
#6484=CARTESIAN_POINT('Origin',(0.,-5.6,4.));
#6485=CARTESIAN_POINT('Origin',(4.25,0.,3.));
#6486=CARTESIAN_POINT('',(-4.25,-5.20474889637625E-16,3.));
#6487=CARTESIAN_POINT('Origin',(0.,0.,3.));
#6488=CARTESIAN_POINT('Origin',(0.,0.,4.5));
#6489=CARTESIAN_POINT('',(-4.25,-5.20474889637625E-16,6.));
#6490=CARTESIAN_POINT('',(-4.25,-5.20474889637625E-16,4.5));
#6491=CARTESIAN_POINT('Origin',(0.,0.,6.));
#6492=CARTESIAN_POINT('Origin',(5.005,0.,6.));
#6493=CARTESIAN_POINT('Origin',(3.,7.,0.));
#6494=CARTESIAN_POINT('',(0.,0.,0.));
#6495=CARTESIAN_POINT('Origin',(11.925,0.,0.));
#6496=CARTESIAN_POINT('',(11.75,-2.515,-3.07998669985559E-16));
#6497=CARTESIAN_POINT('Origin',(11.75,0.,0.));
#6498=CARTESIAN_POINT('',(12.,-2.71857142857143,3.32928979825345E-16));
#6499=CARTESIAN_POINT('',(11.925,-2.6575,-3.25449886873409E-16));
#6500=CARTESIAN_POINT('Origin',(12.,0.,0.));
#6501=CARTESIAN_POINT('Origin',(-0.925,0.,0.));
#6502=CARTESIAN_POINT('',(-1.,-2.71857142857143,-3.32928979825345E-16));
#6503=CARTESIAN_POINT('Origin',(-1.,0.,0.));
#6504=CARTESIAN_POINT('',(-0.75,-2.515,-3.07998669985559E-16));
#6505=CARTESIAN_POINT('',(-0.925,-2.6575,-3.25449886873409E-16));
#6506=CARTESIAN_POINT('Origin',(-0.750000000000001,0.,0.));
#6507=CARTESIAN_POINT('Origin',(5.5,0.,0.));
#6508=CARTESIAN_POINT('',(5.5,-2.515,-3.07998669985559E-16));
#6509=CARTESIAN_POINT('Origin',(-1.,3.7,0.));
#6510=CARTESIAN_POINT('',(-1.,-3.7,-4.53119315684521E-16));
#6511=CARTESIAN_POINT('Origin',(-1.,0.,0.));
#6512=CARTESIAN_POINT('Origin',(-0.900000000000001,0.,0.));
#6513=CARTESIAN_POINT('',(-0.800000000000001,-4.,-4.89858719658941E-16));
#6514=CARTESIAN_POINT('Origin',(-0.800000000000001,0.,0.));
#6515=CARTESIAN_POINT('',(-0.900000000000001,-3.85,-4.71489017671731E-16));
#6516=CARTESIAN_POINT('Origin',(-0.5,0.,0.));
#6517=CARTESIAN_POINT('',(-0.2,-4.,-4.89858719658941E-16));
#6518=CARTESIAN_POINT('Origin',(-0.2,0.,0.));
#6519=CARTESIAN_POINT('',(-0.5,-4.,-4.89858719658941E-16));
#6520=CARTESIAN_POINT('Origin',(-0.1,0.,0.));
#6521=CARTESIAN_POINT('',(1.73472347597681E-17,-3.8,-4.65365783675994E-16));
#6522=CARTESIAN_POINT('Origin',(0.,0.,0.));
#6523=CARTESIAN_POINT('',(-0.1,-3.9,-4.77612251667468E-16));
#6524=CARTESIAN_POINT('Origin',(0.,3.,0.));
#6525=CARTESIAN_POINT('',(0.,-3.,-3.67394039744206E-16));
#6526=CARTESIAN_POINT('Origin',(0.,0.,0.));
#6527=CARTESIAN_POINT('Origin',(5.85,0.,0.));
#6528=CARTESIAN_POINT('',(11.7,-3.,-3.67394039744206E-16));
#6529=CARTESIAN_POINT('Origin',(11.7,0.,0.));
#6530=CARTESIAN_POINT('',(5.85,-3.,-3.67394039744206E-16));
#6531=CARTESIAN_POINT('Origin',(11.85,0.,0.));
#6532=CARTESIAN_POINT('',(12.,-2.8,-3.42901103761259E-16));
#6533=CARTESIAN_POINT('Origin',(12.,0.,0.));
#6534=CARTESIAN_POINT('',(11.85,-2.9,-3.55147571752732E-16));
#6535=CARTESIAN_POINT('Origin',(12.,2.515,0.));
#6536=CARTESIAN_POINT('',(0.,0.,0.));
#6537=CARTESIAN_POINT('Origin',(0.1,0.,0.));
#6538=CARTESIAN_POINT('',(0.2,-3.85,-4.71489017671731E-16));
#6539=CARTESIAN_POINT('Origin',(0.2,0.,0.));
#6540=CARTESIAN_POINT('',(-3.46944695195361E-17,-3.8,-4.65365783675994E-16));
#6541=CARTESIAN_POINT('',(0.1,-3.825,-4.68427400673863E-16));
#6542=CARTESIAN_POINT('Origin',(0.,0.,0.));
#6543=CARTESIAN_POINT('Origin',(0.2,4.25,0.));
#6544=CARTESIAN_POINT('',(0.2,-4.25,-5.20474889637625E-16));
#6545=CARTESIAN_POINT('Origin',(0.2,0.,0.));
#6546=CARTESIAN_POINT('Origin',(0.1,0.,0.));
#6547=CARTESIAN_POINT('',(-5.20417042793042E-17,-4.3,-5.26598123633362E-16));
#6548=CARTESIAN_POINT('',(0.1,-4.275,-5.23536506635494E-16));
#6549=CARTESIAN_POINT('Origin',(0.,0.,0.));
#6550=CARTESIAN_POINT('Origin',(0.,4.85,0.));
#6551=CARTESIAN_POINT('',(-1.64798730217797E-16,-4.85,-5.93953697586466E-16));
#6552=CARTESIAN_POINT('Origin',(0.,0.,0.));
#6553=CARTESIAN_POINT('Origin',(0.075,0.,0.));
#6554=CARTESIAN_POINT('',(0.15,-5.,-6.12323399573677E-16));
#6555=CARTESIAN_POINT('Origin',(0.15,0.,0.));
#6556=CARTESIAN_POINT('',(0.075,-4.925,-6.03138548580071E-16));
#6557=CARTESIAN_POINT('Origin',(1.5,0.,0.));
#6558=CARTESIAN_POINT('',(2.85,-5.,-6.12323399573677E-16));
#6559=CARTESIAN_POINT('Origin',(2.85,0.,0.));
#6560=CARTESIAN_POINT('',(1.5,-5.,-6.12323399573677E-16));
#6561=CARTESIAN_POINT('Origin',(2.925,0.,0.));
#6562=CARTESIAN_POINT('',(3.,-4.85,-5.93953697586466E-16));
#6563=CARTESIAN_POINT('Origin',(3.,0.,0.));
#6564=CARTESIAN_POINT('',(2.925,-4.925,-6.03138548580071E-16));
#6565=CARTESIAN_POINT('Origin',(3.,4.3,0.));
#6566=CARTESIAN_POINT('',(3.,-4.3,-5.26598123633362E-16));
#6567=CARTESIAN_POINT('Origin',(3.,0.,0.));
#6568=CARTESIAN_POINT('Origin',(2.9,0.,0.));
#6569=CARTESIAN_POINT('',(2.8,-4.25,-5.20474889637625E-16));
#6570=CARTESIAN_POINT('',(2.9,-4.275,-5.23536506635494E-16));
#6571=CARTESIAN_POINT('Origin',(2.8,0.,0.));
#6572=CARTESIAN_POINT('Origin',(2.8,3.85,0.));
#6573=CARTESIAN_POINT('',(2.8,-3.85,-4.71489017671731E-16));
#6574=CARTESIAN_POINT('Origin',(2.8,0.,0.));
#6575=CARTESIAN_POINT('Origin',(2.9,0.,0.));
#6576=CARTESIAN_POINT('',(3.,-3.8,-4.65365783675994E-16));
#6577=CARTESIAN_POINT('Origin',(3.,0.,0.));
#6578=CARTESIAN_POINT('',(2.9,-3.825,-4.68427400673863E-16));
#6579=CARTESIAN_POINT('Origin',(3.,3.15,0.));
#6580=CARTESIAN_POINT('',(3.,-3.15,-3.85763741731416E-16));
#6581=CARTESIAN_POINT('Origin',(3.,0.,0.));
#6582=CARTESIAN_POINT('Origin',(2.925,0.,0.));
#6583=CARTESIAN_POINT('',(2.85,-3.,-3.67394039744206E-16));
#6584=CARTESIAN_POINT('',(2.925,-3.075,-3.76578890737811E-16));
#6585=CARTESIAN_POINT('Origin',(2.85,0.,0.));
#6586=CARTESIAN_POINT('Origin',(1.5,0.,0.));
#6587=CARTESIAN_POINT('',(0.15,-3.,-3.67394039744206E-16));
#6588=CARTESIAN_POINT('',(1.5,-3.,-3.67394039744206E-16));
#6589=CARTESIAN_POINT('Origin',(0.15,0.,0.));
#6590=CARTESIAN_POINT('Origin',(0.075,0.,0.));
#6591=CARTESIAN_POINT('',(-3.46944695195361E-17,-3.15,-3.85763741731416E-16));
#6592=CARTESIAN_POINT('',(0.075,-3.075,-3.76578890737811E-16));
#6593=CARTESIAN_POINT('Origin',(0.,0.,0.));
#6594=CARTESIAN_POINT('Origin',(0.,3.8,0.));
#6595=CARTESIAN_POINT('',(0.,0.,0.));
#6596=CARTESIAN_POINT('Origin',(0.25,0.,0.));
#6597=CARTESIAN_POINT('',(0.5,-3.05,-3.73517273739943E-16));
#6598=CARTESIAN_POINT('Origin',(0.5,0.,0.));
#6599=CARTESIAN_POINT('',(0.,-3.05,-3.73517273739943E-16));
#6600=CARTESIAN_POINT('',(0.25,-3.05,-3.73517273739943E-16));
#6601=CARTESIAN_POINT('Origin',(0.,0.,0.));
#6602=CARTESIAN_POINT('Origin',(0.,4.,0.));
#6603=CARTESIAN_POINT('',(0.,-4.,-4.89858719658941E-16));
#6604=CARTESIAN_POINT('Origin',(0.,0.,0.));
#6605=CARTESIAN_POINT('Origin',(0.25,0.,0.));
#6606=CARTESIAN_POINT('',(0.5,-4.,-4.89858719658941E-16));
#6607=CARTESIAN_POINT('Origin',(0.5,0.,0.));
#6608=CARTESIAN_POINT('',(0.25,-4.,-4.89858719658941E-16));
#6609=CARTESIAN_POINT('Origin',(0.5,3.05,0.));
#6610=CARTESIAN_POINT('',(0.,0.,0.));
#6611=CARTESIAN_POINT('Origin',(2.47436860633172,-2.3,11.9));
#6612=CARTESIAN_POINT('',(4.7116875957559,-2.2,12.));
#6613=CARTESIAN_POINT('',(4.83735464897913,-2.4,11.8));
#6614=CARTESIAN_POINT('Ctrl Pts',(4.83735464897913,-2.4,11.8));
#6615=CARTESIAN_POINT('Ctrl Pts',(4.77452112236735,-2.29868398264425,11.9013160173557));
#6616=CARTESIAN_POINT('Ctrl Pts',(4.7116875957559,-2.2,12.));
#6617=CARTESIAN_POINT('',(10.37211794039,-2.4,11.8));
#6618=CARTESIAN_POINT('',(2.47436860633172,-2.4,11.8));
#6619=CARTESIAN_POINT('',(10.4347524157501,-2.2,12.));
#6620=CARTESIAN_POINT('Ctrl Pts',(10.4347524157501,-2.2,12.));
#6621=CARTESIAN_POINT('Ctrl Pts',(10.4034351780701,-2.29803846124815,11.9019615387518));
#6622=CARTESIAN_POINT('Ctrl Pts',(10.37211794039,-2.4,11.8));
#6623=CARTESIAN_POINT('',(2.47436860633172,-2.2,12.));
#6624=CARTESIAN_POINT('Origin',(4.94873721266345,-2.4,9.5));
#6625=CARTESIAN_POINT('',(4.94873721266345,-2.4,11.7));
#6626=CARTESIAN_POINT('Ctrl Pts',(4.83735464897798,-2.4,11.800000000001));
#6627=CARTESIAN_POINT('Ctrl Pts',(4.89253500162966,-2.4,11.7505690860322));
#6628=CARTESIAN_POINT('Ctrl Pts',(4.94873721266345,-2.4,11.7));
#6629=CARTESIAN_POINT('',(4.94873721266345,-2.4,9.7));
#6630=CARTESIAN_POINT('',(4.94873721266345,-2.4,9.5));
#6631=CARTESIAN_POINT('',(10.2,-2.4,9.7));
#6632=CARTESIAN_POINT('',(2.47436860633172,-2.4,9.7));
#6633=CARTESIAN_POINT('',(10.2,-2.4,11.7));
#6634=CARTESIAN_POINT('',(10.2,-2.4,9.5));
#6635=CARTESIAN_POINT('Ctrl Pts',(10.2,-2.4,11.7));
#6636=CARTESIAN_POINT('Ctrl Pts',(10.2875175968085,-2.4,11.7525105580851));
#6637=CARTESIAN_POINT('Ctrl Pts',(10.37211794039,-2.4,11.8));
#6638=CARTESIAN_POINT('Origin',(-5.1,-2.3,11.9));
#6639=CARTESIAN_POINT('',(-10.4347524157501,-2.2,12.));
#6640=CARTESIAN_POINT('',(-10.37211794039,-2.4,11.8));
#6641=CARTESIAN_POINT('Ctrl Pts',(-10.37211794039,-2.4,11.8));
#6642=CARTESIAN_POINT('Ctrl Pts',(-10.4034351780701,-2.29803846124801,11.901961538752));
#6643=CARTESIAN_POINT('Ctrl Pts',(-10.4347524157501,-2.2,12.));
#6644=CARTESIAN_POINT('',(-4.83735464897913,-2.4,11.8));
#6645=CARTESIAN_POINT('',(-5.1,-2.4,11.8));
#6646=CARTESIAN_POINT('',(-4.7116875957559,-2.2,12.));
#6647=CARTESIAN_POINT('Ctrl Pts',(-4.7116875957559,-2.2,12.));
#6648=CARTESIAN_POINT('Ctrl Pts',(-4.7745211223673,-2.29868398264418,11.9013160173558));
#6649=CARTESIAN_POINT('Ctrl Pts',(-4.83735464897913,-2.4,11.8));
#6650=CARTESIAN_POINT('',(-5.1,-2.2,12.));
#6651=CARTESIAN_POINT('Origin',(-10.2,-2.4,9.5));
#6652=CARTESIAN_POINT('',(-10.2,-2.4,11.7));
#6653=CARTESIAN_POINT('Ctrl Pts',(-10.37211794039,-2.4,11.8));
#6654=CARTESIAN_POINT('Ctrl Pts',(-10.2875175968085,-2.4,11.7525105580851));
#6655=CARTESIAN_POINT('Ctrl Pts',(-10.2,-2.4,11.7));
#6656=CARTESIAN_POINT('',(-10.2,-2.4,9.7));
#6657=CARTESIAN_POINT('',(-10.2,-2.4,9.5));
#6658=CARTESIAN_POINT('',(-4.94873721266345,-2.4,9.7));
#6659=CARTESIAN_POINT('',(-5.1,-2.4,9.7));
#6660=CARTESIAN_POINT('',(-4.94873721266345,-2.4,11.7));
#6661=CARTESIAN_POINT('',(-4.94873721266345,-2.4,9.5));
#6662=CARTESIAN_POINT('Ctrl Pts',(-4.94873721266345,-2.4,11.7));
#6663=CARTESIAN_POINT('Ctrl Pts',(-4.89253500163078,-2.4,11.7505690860312));
#6664=CARTESIAN_POINT('Ctrl Pts',(-4.83735464898018,-2.4,11.7999999999991));
#6665=CARTESIAN_POINT('Origin',(-2.47436860633172,2.3,11.9));
#6666=CARTESIAN_POINT('',(-4.7116875957559,2.2,12.));
#6667=CARTESIAN_POINT('',(-4.83735464897913,2.4,11.8));
#6668=CARTESIAN_POINT('Ctrl Pts',(-4.83735464897913,2.4,11.8));
#6669=CARTESIAN_POINT('Ctrl Pts',(-4.7745211223673,2.29868398264418,11.9013160173558));
#6670=CARTESIAN_POINT('Ctrl Pts',(-4.7116875957559,2.2,12.));
#6671=CARTESIAN_POINT('',(-10.37211794039,2.4,11.8));
#6672=CARTESIAN_POINT('',(-2.47436860633172,2.4,11.8));
#6673=CARTESIAN_POINT('',(-10.4347524157501,2.2,12.));
#6674=CARTESIAN_POINT('Ctrl Pts',(-10.4347524157501,2.2,12.));
#6675=CARTESIAN_POINT('Ctrl Pts',(-10.4034351780701,2.29803846124801,11.901961538752));
#6676=CARTESIAN_POINT('Ctrl Pts',(-10.37211794039,2.4,11.8));
#6677=CARTESIAN_POINT('',(-2.47436860633172,2.2,12.));
#6678=CARTESIAN_POINT('Origin',(-4.94873721266345,2.4,9.5));
#6679=CARTESIAN_POINT('',(-4.94873721266345,2.4,11.7));
#6680=CARTESIAN_POINT('Ctrl Pts',(-4.83735464897788,2.4,11.8000000000011));
#6681=CARTESIAN_POINT('Ctrl Pts',(-4.89253500162949,2.4,11.7505690860323));
#6682=CARTESIAN_POINT('Ctrl Pts',(-4.94873721266345,2.4,11.7));
#6683=CARTESIAN_POINT('',(-4.94873721266345,2.4,9.7));
#6684=CARTESIAN_POINT('',(-4.94873721266345,2.4,9.5));
#6685=CARTESIAN_POINT('',(-10.2,2.4,9.7));
#6686=CARTESIAN_POINT('',(-2.47436860633172,2.4,9.7));
#6687=CARTESIAN_POINT('',(-10.2,2.4,11.7));
#6688=CARTESIAN_POINT('',(-10.2,2.4,9.5));
#6689=CARTESIAN_POINT('Ctrl Pts',(-10.2,2.4,11.7));
#6690=CARTESIAN_POINT('Ctrl Pts',(-10.2875175968085,2.4,11.7525105580851));
#6691=CARTESIAN_POINT('Ctrl Pts',(-10.37211794039,2.4,11.8));
#6692=CARTESIAN_POINT('Origin',(5.1,2.3,11.9));
#6693=CARTESIAN_POINT('',(10.4347524157501,2.2,12.));
#6694=CARTESIAN_POINT('',(10.37211794039,2.4,11.8));
#6695=CARTESIAN_POINT('Ctrl Pts',(10.37211794039,2.4,11.8));
#6696=CARTESIAN_POINT('Ctrl Pts',(10.4034351780701,2.29803846124801,11.901961538752));
#6697=CARTESIAN_POINT('Ctrl Pts',(10.4347524157501,2.2,12.));
#6698=CARTESIAN_POINT('',(4.83735464897913,2.4,11.8));
#6699=CARTESIAN_POINT('',(5.1,2.4,11.8));
#6700=CARTESIAN_POINT('',(4.7116875957559,2.2,12.));
#6701=CARTESIAN_POINT('Ctrl Pts',(4.7116875957559,2.2,12.));
#6702=CARTESIAN_POINT('Ctrl Pts',(4.7745211223673,2.29868398264418,11.9013160173558));
#6703=CARTESIAN_POINT('Ctrl Pts',(4.83735464897913,2.4,11.8));
#6704=CARTESIAN_POINT('',(5.1,2.2,12.));
#6705=CARTESIAN_POINT('Origin',(10.2,2.4,9.5));
#6706=CARTESIAN_POINT('',(10.2,2.4,11.7));
#6707=CARTESIAN_POINT('Ctrl Pts',(10.37211794039,2.4,11.8));
#6708=CARTESIAN_POINT('Ctrl Pts',(10.2875175968085,2.4,11.7525105580851));
#6709=CARTESIAN_POINT('Ctrl Pts',(10.2,2.4,11.7));
#6710=CARTESIAN_POINT('',(10.2,2.4,9.7));
#6711=CARTESIAN_POINT('',(10.2,2.4,9.5));
#6712=CARTESIAN_POINT('',(4.94873721266345,2.4,9.7));
#6713=CARTESIAN_POINT('',(5.1,2.4,9.7));
#6714=CARTESIAN_POINT('',(4.94873721266345,2.4,11.7));
#6715=CARTESIAN_POINT('',(4.94873721266345,2.4,9.5));
#6716=CARTESIAN_POINT('Ctrl Pts',(4.94873721497344,2.4,11.6999999979215));
#6717=CARTESIAN_POINT('Ctrl Pts',(4.89253500276439,2.4,11.7505690850157));
#6718=CARTESIAN_POINT('Ctrl Pts',(4.83735464898018,2.4,11.7999999999991));
#6719=CARTESIAN_POINT('Origin',(-5.1,-2.3,9.6));
#6720=CARTESIAN_POINT('',(-10.2679491924311,-2.2,9.5));
#6721=CARTESIAN_POINT('',(-4.82182538049648,-2.2,9.5));
#6722=CARTESIAN_POINT('',(-5.1,-2.2,9.5));
#6723=CARTESIAN_POINT('Ctrl Pts',(-4.82182538049648,-2.2,9.5));
#6724=CARTESIAN_POINT('Ctrl Pts',(-4.86458548124608,-2.26651023840872,9.56651023840872));
#6725=CARTESIAN_POINT('Ctrl Pts',(-4.90689191151574,-2.33319954872105,9.63319954872104));
#6726=CARTESIAN_POINT('Ctrl Pts',(-4.94873721266345,-2.4,9.7));
#6727=CARTESIAN_POINT('Ctrl Pts',(-10.2679491924311,-2.2,9.5));
#6728=CARTESIAN_POINT('Ctrl Pts',(-10.2448893867531,-2.26656792507827,9.56656792507827));
#6729=CARTESIAN_POINT('Ctrl Pts',(-10.2222358749559,-2.3332923751323,9.6332923751323));
#6730=CARTESIAN_POINT('Ctrl Pts',(-10.2,-2.4,9.7));
#6731=CARTESIAN_POINT('Origin',(0.,0.,9.6));
#6732=CARTESIAN_POINT('',(4.82182538049648,-2.2,9.5));
#6733=CARTESIAN_POINT('Origin',(0.,0.,9.5));
#6734=CARTESIAN_POINT('Ctrl Pts',(4.82182538049648,-2.2,9.5));
#6735=CARTESIAN_POINT('Ctrl Pts',(4.86458548124613,-2.26651023840879,9.56651023840879));
#6736=CARTESIAN_POINT('Ctrl Pts',(4.90689191151583,-2.33319954872119,9.63319954872119));
#6737=CARTESIAN_POINT('Ctrl Pts',(4.94873721266345,-2.4,9.7));
#6738=CARTESIAN_POINT('Origin',(0.,0.,9.7));
#6739=CARTESIAN_POINT('Origin',(12.,0.,9.6));
#6740=CARTESIAN_POINT('Origin',(12.,0.,9.7));
#6741=CARTESIAN_POINT('',(10.2679491924311,-2.2,9.5));
#6742=CARTESIAN_POINT('Ctrl Pts',(10.2,-2.4,9.7));
#6743=CARTESIAN_POINT('Ctrl Pts',(10.2222358749557,-2.33329237513297,9.63329237513297));
#6744=CARTESIAN_POINT('Ctrl Pts',(10.244889386753,-2.26656792507858,9.56656792507857));
#6745=CARTESIAN_POINT('Ctrl Pts',(10.2679491924311,-2.2,9.5));
#6746=CARTESIAN_POINT('',(10.2679491924311,2.2,9.5));
#6747=CARTESIAN_POINT('Origin',(12.,0.,9.5));
#6748=CARTESIAN_POINT('Ctrl Pts',(10.2679491924311,2.2,9.5));
#6749=CARTESIAN_POINT('Ctrl Pts',(10.2448893867531,2.26656792507827,9.56656792507827));
#6750=CARTESIAN_POINT('Ctrl Pts',(10.2222358749559,2.3332923751323,9.6332923751323));
#6751=CARTESIAN_POINT('Ctrl Pts',(10.2,2.4,9.7));
#6752=CARTESIAN_POINT('Origin',(2.47436860633172,-2.3,9.6));
#6753=CARTESIAN_POINT('',(2.47436860633172,-2.2,9.5));
#6754=CARTESIAN_POINT('Origin',(5.1,2.3,9.6));
#6755=CARTESIAN_POINT('',(4.82182538049648,2.2,9.5));
#6756=CARTESIAN_POINT('',(5.1,2.2,9.5));
#6757=CARTESIAN_POINT('Ctrl Pts',(4.82182538049648,2.2,9.5));
#6758=CARTESIAN_POINT('Ctrl Pts',(4.86458548124611,2.26651023840876,9.56651023840876));
#6759=CARTESIAN_POINT('Ctrl Pts',(4.90689191151579,2.33319954872112,9.63319954872112));
#6760=CARTESIAN_POINT('Ctrl Pts',(4.94873721266345,2.4,9.7));
#6761=CARTESIAN_POINT('Origin',(0.,0.,9.6));
#6762=CARTESIAN_POINT('',(0.,5.5,9.7));
#6763=CARTESIAN_POINT('Origin',(0.,0.,9.7));
#6764=CARTESIAN_POINT('Origin',(0.,0.,9.7));
#6765=CARTESIAN_POINT('',(-4.82182538049648,2.2,9.5));
#6766=CARTESIAN_POINT('Origin',(0.,0.,9.5));
#6767=CARTESIAN_POINT('Ctrl Pts',(-4.82182538049648,2.2,9.5));
#6768=CARTESIAN_POINT('Ctrl Pts',(-4.86458548124609,2.26651023840874,9.56651023840873));
#6769=CARTESIAN_POINT('Ctrl Pts',(-4.90689191151576,2.33319954872108,9.63319954872108));
#6770=CARTESIAN_POINT('Ctrl Pts',(-4.94873721266345,2.4,9.7));
#6771=CARTESIAN_POINT('Origin',(-2.47436860633172,2.3,9.6));
#6772=CARTESIAN_POINT('',(-10.2679491924311,2.2,9.5));
#6773=CARTESIAN_POINT('',(-2.47436860633172,2.2,9.5));
#6774=CARTESIAN_POINT('Ctrl Pts',(-10.2679491924311,2.2,9.5));
#6775=CARTESIAN_POINT('Ctrl Pts',(-10.244889386753,2.26656792507857,9.56656792507857));
#6776=CARTESIAN_POINT('Ctrl Pts',(-10.2222358749557,2.33329237513297,9.63329237513297));
#6777=CARTESIAN_POINT('Ctrl Pts',(-10.2,2.4,9.7));
#6778=CARTESIAN_POINT('Origin',(-12.,0.,9.6));
#6779=CARTESIAN_POINT('Origin',(-12.,0.,9.7));
#6780=CARTESIAN_POINT('Origin',(-12.,0.,9.5));
#6781=CARTESIAN_POINT('Origin',(-12.,0.,9.5));
#6782=CARTESIAN_POINT('Origin',(-12.,0.,11.7));
#6783=CARTESIAN_POINT('Origin',(0.,0.,9.5));
#6784=CARTESIAN_POINT('Origin',(0.,0.,11.7));
#6785=CARTESIAN_POINT('Origin',(0.,0.,9.5));
#6786=CARTESIAN_POINT('',(0.447213604330343,5.4817880287459,11.6999999979215));
#6787=CARTESIAN_POINT('Ctrl Pts',(-1.04083408558608E-16,5.5,9.7));
#6788=CARTESIAN_POINT('Ctrl Pts',(0.132186811917676,5.5,9.7));
#6789=CARTESIAN_POINT('Ctrl Pts',(0.272965016647602,5.49475196102956,9.72648386715131));
#6790=CARTESIAN_POINT('Ctrl Pts',(0.531569703786443,5.47578694476791,9.83374194918294));
#6791=CARTESIAN_POINT('Ctrl Pts',(0.649422667404825,5.4623316644562,9.91449842691308));
#6792=CARTESIAN_POINT('Ctrl Pts',(0.835505886786072,5.43697965273112,10.1005816462943));
#6793=CARTESIAN_POINT('Ctrl Pts',(0.91625898403177,5.42341568535631,10.2184327722933));
#6794=CARTESIAN_POINT('Ctrl Pts',(1.02351461335488,5.40420078323371,10.4770310937253));
#6795=CARTESIAN_POINT('Ctrl Pts',(1.05,5.39884246852971,10.6178070593475));
#6796=CARTESIAN_POINT('Ctrl Pts',(1.05,5.39884246852971,10.75));
#6797=CARTESIAN_POINT('Ctrl Pts',(1.05,5.39884246852971,10.8821929406525));
#6798=CARTESIAN_POINT('Ctrl Pts',(1.02351461335488,5.40420078323371,11.0229689062747));
#6799=CARTESIAN_POINT('Ctrl Pts',(0.91625898403177,5.42341568535631,11.2815672277067));
#6800=CARTESIAN_POINT('Ctrl Pts',(0.835505886786072,5.43697965273112,11.3994183537057));
#6801=CARTESIAN_POINT('Ctrl Pts',(0.660316211845406,5.46084752597609,11.5746080286463));
#6802=CARTESIAN_POINT('Ctrl Pts',(0.558936689613752,5.47267346917065,11.6474062234574));
#6803=CARTESIAN_POINT('Ctrl Pts',(0.447213603533743,5.48178802881089,11.6999999962181));
#6804=CARTESIAN_POINT('Origin',(0.,0.,11.7));
#6805=CARTESIAN_POINT('Origin',(12.,0.,9.5));
#6806=CARTESIAN_POINT('Origin',(12.,0.,11.7));
#6807=CARTESIAN_POINT('Origin',(0.,0.,9.5));
#6808=CARTESIAN_POINT('',(-3.01,-3.68618686543353E-16,9.5));
#6809=CARTESIAN_POINT('Origin',(0.,0.,9.5));
#6810=CARTESIAN_POINT('',(10.48,-1.86146313470398E-16,9.5));
#6811=CARTESIAN_POINT('Origin',(12.,0.,9.5));
#6812=CARTESIAN_POINT('',(-13.52,-1.86146313470398E-16,9.5));
#6813=CARTESIAN_POINT('Origin',(-12.,0.,9.5));
#6814=CARTESIAN_POINT('Origin',(12.,0.,11.85));
#6815=CARTESIAN_POINT('Origin',(12.,0.,12.));
#6816=CARTESIAN_POINT('Origin',(0.,0.,11.85));
#6817=CARTESIAN_POINT('',(-0.447213604330343,5.4817880287459,11.6999999979215));
#6818=CARTESIAN_POINT('Ctrl Pts',(0.447213602432565,5.4817880321751,11.6999999967365));
#6819=CARTESIAN_POINT('Ctrl Pts',(0.414910948534785,5.46916630571322,11.7152065085969));
#6820=CARTESIAN_POINT('Ctrl Pts',(0.381292409563767,5.45779439913161,11.7290076072377));
#6821=CARTESIAN_POINT('Ctrl Pts',(0.235875663864367,5.41607161270286,11.7798828268936));
#6822=CARTESIAN_POINT('Ctrl Pts',(0.114682100258675,5.4,11.8));
#6823=CARTESIAN_POINT('Ctrl Pts',(-0.114682100258675,5.4,11.8));
#6824=CARTESIAN_POINT('Ctrl Pts',(-0.235875663864366,5.41607161270286,11.7798828268936));
#6825=CARTESIAN_POINT('Ctrl Pts',(-0.381292409563766,5.45779439913161,11.7290076072377));
#6826=CARTESIAN_POINT('Ctrl Pts',(-0.414910948534784,5.46916630571322,11.7152065085969));
#6827=CARTESIAN_POINT('Ctrl Pts',(-0.447213602432565,5.4817880321751,11.6999999967365));
#6828=CARTESIAN_POINT('Origin',(0.,0.,11.7));
#6829=CARTESIAN_POINT('Origin',(0.,0.,12.));
#6830=CARTESIAN_POINT('Origin',(0.,0.,9.5));
#6831=CARTESIAN_POINT('',(-1.05,5.39884246852971,10.75));
#6832=CARTESIAN_POINT('Ctrl Pts',(-0.447213603533744,5.48178802881089,11.6999999962181));
#6833=CARTESIAN_POINT('Ctrl Pts',(-0.558936689613753,5.47267346917065,11.6474062234574));
#6834=CARTESIAN_POINT('Ctrl Pts',(-0.660316211845406,5.46084752597609,11.5746080286463));
#6835=CARTESIAN_POINT('Ctrl Pts',(-0.835505886786072,5.43697965273112,11.3994183537057));
#6836=CARTESIAN_POINT('Ctrl Pts',(-0.91625898403177,5.42341568535631,11.2815672277067));
#6837=CARTESIAN_POINT('Ctrl Pts',(-1.02351461335488,5.40420078323371,11.0229689062747));
#6838=CARTESIAN_POINT('Ctrl Pts',(-1.05,5.39884246852971,10.8821929406525));
#6839=CARTESIAN_POINT('Ctrl Pts',(-1.05,5.39884246852971,10.75));
#6840=CARTESIAN_POINT('Ctrl Pts',(-1.05,5.39884246852971,10.75));
#6841=CARTESIAN_POINT('Ctrl Pts',(-1.05,5.39884246852971,10.6178070593475));
#6842=CARTESIAN_POINT('Ctrl Pts',(-1.02351461335488,5.40420078323371,10.4770310937253));
#6843=CARTESIAN_POINT('Ctrl Pts',(-0.91625898403177,5.42341568535631,10.2184327722933));
#6844=CARTESIAN_POINT('Ctrl Pts',(-0.835505886786073,5.43697965273112,10.1005816462943));
#6845=CARTESIAN_POINT('Ctrl Pts',(-0.649422667404826,5.4623316644562,9.91449842691308));
#6846=CARTESIAN_POINT('Ctrl Pts',(-0.531569703786443,5.47578694476791,9.83374194918294));
#6847=CARTESIAN_POINT('Ctrl Pts',(-0.272965016647603,5.49475196102956,9.72648386715131));
#6848=CARTESIAN_POINT('Ctrl Pts',(-0.132186811917677,5.5,9.7));
#6849=CARTESIAN_POINT('Ctrl Pts',(-1.73472347597681E-16,5.5,9.7));
#6850=CARTESIAN_POINT('Origin',(0.,5.5,10.75));
#6851=CARTESIAN_POINT('',(-1.05,2.9,10.75));
#6852=CARTESIAN_POINT('',(-1.05,5.5,10.75));
#6853=CARTESIAN_POINT('',(-0.806287789812048,2.9,10.077393131168));
#6854=CARTESIAN_POINT('Origin',(0.,2.9,10.75));
#6855=CARTESIAN_POINT('',(0.806287789812048,2.9,10.077393131168));
#6856=CARTESIAN_POINT('Ctrl Pts',(0.806287789812047,2.9,10.077393131168));
#6857=CARTESIAN_POINT('Ctrl Pts',(0.785808654937835,2.90569381944655,10.0528437589267));
#6858=CARTESIAN_POINT('Ctrl Pts',(0.76444442856579,2.91139815952389,10.029520188074));
#6859=CARTESIAN_POINT('Ctrl Pts',(0.649888518401964,2.94055606794566,9.91496427791022));
#6860=CARTESIAN_POINT('Ctrl Pts',(0.53255794166538,2.96538003783021,9.83432362785116));
#6861=CARTESIAN_POINT('Ctrl Pts',(0.274166742773895,3.00032153730045,9.72681194070543));
#6862=CARTESIAN_POINT('Ctrl Pts',(0.133022354666825,3.01,9.7));
#6863=CARTESIAN_POINT('Ctrl Pts',(-0.133022354666825,3.01,9.7));
#6864=CARTESIAN_POINT('Ctrl Pts',(-0.274166742773895,3.00032153730045,9.72681194070543));
#6865=CARTESIAN_POINT('Ctrl Pts',(-0.53255794166538,2.96538003783021,9.83432362785116));
#6866=CARTESIAN_POINT('Ctrl Pts',(-0.649888518401964,2.94055606794566,9.91496427791022));
#6867=CARTESIAN_POINT('Ctrl Pts',(-0.76444442856579,2.91139815952389,10.029520188074));
#6868=CARTESIAN_POINT('Ctrl Pts',(-0.785808654937835,2.90569381944655,10.0528437589267));
#6869=CARTESIAN_POINT('Ctrl Pts',(-0.806287789812047,2.9,10.077393131168));
#6870=CARTESIAN_POINT('',(0.806287789812048,2.9,11.422606868832));
#6871=CARTESIAN_POINT('Origin',(0.,2.9,10.75));
#6872=CARTESIAN_POINT('',(0.44721360294724,2.97659200988966,11.6999999982471));
#6873=CARTESIAN_POINT('Ctrl Pts',(0.447213602284006,2.9765920099893,11.6999999968064));
#6874=CARTESIAN_POINT('Ctrl Pts',(0.559174059233342,2.9597706790519,11.6472944816127));
#6875=CARTESIAN_POINT('Ctrl Pts',(0.660473235012751,2.93786194070974,11.574451005479));
#6876=CARTESIAN_POINT('Ctrl Pts',(0.76444442856579,2.91139815952389,11.470479811926));
#6877=CARTESIAN_POINT('Ctrl Pts',(0.785808654937837,2.90569381944655,11.4471562410733));
#6878=CARTESIAN_POINT('Ctrl Pts',(0.806287789812047,2.9,11.422606868832));
#6879=CARTESIAN_POINT('',(-0.44721360294724,2.97659200988966,11.6999999982471));
#6880=CARTESIAN_POINT('Ctrl Pts',(-0.447213601060151,2.97659200752633,11.6999999973825));
#6881=CARTESIAN_POINT('Ctrl Pts',(-0.390045315290127,3.01239525686365,11.7269120342416));
#6882=CARTESIAN_POINT('Ctrl Pts',(-0.324286474226429,3.04489074102158,11.7512712452848));
#6883=CARTESIAN_POINT('Ctrl Pts',(-0.171947398222887,3.09567084784442,11.7892957080173));
#6884=CARTESIAN_POINT('Ctrl Pts',(-0.0834561363660907,3.11,11.8));
#6885=CARTESIAN_POINT('Ctrl Pts',(0.0834561363660904,3.11,11.8));
#6886=CARTESIAN_POINT('Ctrl Pts',(0.171947398222886,3.09567084784442,11.7892957080173));
#6887=CARTESIAN_POINT('Ctrl Pts',(0.324286474226428,3.04489074102158,11.7512712452848));
#6888=CARTESIAN_POINT('Ctrl Pts',(0.390045315290127,3.01239525686365,11.7269120342416));
#6889=CARTESIAN_POINT('Ctrl Pts',(0.447213601060151,2.97659200752634,11.6999999973825));
#6890=CARTESIAN_POINT('',(-0.806287789812048,2.9,11.422606868832));
#6891=CARTESIAN_POINT('Ctrl Pts',(-0.806287789812047,2.9,11.422606868832));
#6892=CARTESIAN_POINT('Ctrl Pts',(-0.785808654937835,2.90569381944655,11.4471562410733));
#6893=CARTESIAN_POINT('Ctrl Pts',(-0.76444442856579,2.91139815952389,11.470479811926));
#6894=CARTESIAN_POINT('Ctrl Pts',(-0.66047323501275,2.93786194070974,11.574451005479));
#6895=CARTESIAN_POINT('Ctrl Pts',(-0.559174059233342,2.9597706790519,11.6472944816127));
#6896=CARTESIAN_POINT('Ctrl Pts',(-0.447213602284006,2.9765920099893,11.6999999968064));
#6897=CARTESIAN_POINT('Origin',(0.,2.9,10.75));
#6898=CARTESIAN_POINT('Origin',(-12.,0.,11.85));
#6899=CARTESIAN_POINT('Origin',(-12.,0.,12.));
#6900=CARTESIAN_POINT('Origin',(0.,0.,11.85));
#6901=CARTESIAN_POINT('Origin',(0.,0.,12.));
#6902=CARTESIAN_POINT('Origin',(0.,0.,11.85));
#6903=CARTESIAN_POINT('',(-3.31,-4.05358090517774E-16,12.));
#6904=CARTESIAN_POINT('Origin',(0.,0.,12.));
#6905=CARTESIAN_POINT('',(-3.00999999738253,-3.68618686222806E-16,11.6999999973825));
#6906=CARTESIAN_POINT('',(-3.16,-3.86988388530564E-16,11.85));
#6907=CARTESIAN_POINT('Origin',(0.,0.,11.7));
#6908=CARTESIAN_POINT('Origin',(0.,0.,11.7));
#6909=CARTESIAN_POINT('Origin',(0.,0.,12.));
#6910=CARTESIAN_POINT('',(10.48,-1.86146313470398E-16,12.));
#6911=CARTESIAN_POINT('Origin',(12.,0.,12.));
#6912=CARTESIAN_POINT('',(-13.52,-1.86146313470398E-16,12.));
#6913=CARTESIAN_POINT('Origin',(-12.,0.,12.));
#6914=CARTESIAN_POINT('Origin',(0.,2.9,10.75));
#6915=CARTESIAN_POINT('',(-0.806287789812048,2.9,12.));
#6916=CARTESIAN_POINT('Origin',(0.,2.9,10.75));
#6917=CARTESIAN_POINT('',(0.806287789812048,2.9,12.));
#6918=CARTESIAN_POINT('Origin',(-12.,0.,12.));
#6919=CARTESIAN_POINT('',(-13.52,1.86146313470398E-16,12.));
#6920=CARTESIAN_POINT('Origin',(12.,0.,12.));
#6921=CARTESIAN_POINT('',(10.48,1.86146313470398E-16,12.));
#6922=CARTESIAN_POINT('Origin',(0.,0.,12.));
#6923=CARTESIAN_POINT('',(-3.01,3.68618686543353E-16,12.));
#6924=CARTESIAN_POINT('',(0.,0.,0.));
#6925=CARTESIAN_POINT('Origin',(1.25,0.,0.));
#6926=CARTESIAN_POINT('',(0.295735916889676,-0.96799567585261,0.000586695936425057));
#6927=CARTESIAN_POINT('',(0.237764083110324,-0.96769285498825,0.00103535076607003));
#6928=CARTESIAN_POINT('',(1.25,-0.96675,-1.1839272930757E-16));
#6929=CARTESIAN_POINT('',(0.16675,0.425622873836743,0.868928367815379));
#6930=CARTESIAN_POINT('Ctrl Pts',(0.295735916889676,-0.96799567585261,0.000586695936425057));
#6931=CARTESIAN_POINT('Ctrl Pts',(0.29377460420558,-0.968188204818438,0.0302592824465942));
#6932=CARTESIAN_POINT('Ctrl Pts',(0.291813291521485,-0.966943036624424,
0.0599143163822494));
#6933=CARTESIAN_POINT('Ctrl Pts',(0.289851978837389,-0.964207634563732,
0.0894298058826106));
#6934=CARTESIAN_POINT('Ctrl Pts',(0.268635853616945,-0.934617945413966,
0.4087079741524));
#6935=CARTESIAN_POINT('Ctrl Pts',(0.247419728396501,-0.730649773407094,
0.711657465788388));
#6936=CARTESIAN_POINT('Ctrl Pts',(0.226203603176058,-0.445967050164715,
0.859445316294661));
#6937=CARTESIAN_POINT('Ctrl Pts',(0.206385735450705,-0.180046459373982,
0.997493147475694));
#6938=CARTESIAN_POINT('Ctrl Pts',(0.186567867725353,0.156300216529493,1.00015737338151));
#6939=CARTESIAN_POINT('Ctrl Pts',(0.16675,0.426126619158378,0.869594511950287));
#6940=CARTESIAN_POINT('',(0.16675,-0.425119128515107,0.868262223680471));
#6941=CARTESIAN_POINT('Origin',(0.16675,0.,0.));
#6942=CARTESIAN_POINT('Ctrl Pts',(0.16675,-0.425119128515108,0.868262223680471));
#6943=CARTESIAN_POINT('Ctrl Pts',(0.187966125220444,-0.714478034118649,
0.726586123507843));
#6944=CARTESIAN_POINT('Ctrl Pts',(0.209182250440888,-0.924905046764807,
0.430096049228702));
#6945=CARTESIAN_POINT('Ctrl Pts',(0.230398375661332,-0.961770620498793,
0.112067875014351));
#6946=CARTESIAN_POINT('Ctrl Pts',(0.232853611477663,-0.966036888541652,
0.0752640686727022));
#6947=CARTESIAN_POINT('Ctrl Pts',(0.235308847293994,-0.967978774477045,
0.0381718182248514));
#6948=CARTESIAN_POINT('Ctrl Pts',(0.237764083110324,-0.96769285498825,0.00103535076607003));
#6949=CARTESIAN_POINT('Origin',(1.25,0.,0.));
#6950=CARTESIAN_POINT('',(0.695735916889677,-0.965535960161722,0.000603907848525584));
#6951=CARTESIAN_POINT('',(0.637764083110324,-0.965403356746268,0.000512007511799884));
#6952=CARTESIAN_POINT('',(1.25,-0.96675,-1.1839272930757E-16));
#6953=CARTESIAN_POINT('Ctrl Pts',(0.695735916889677,-0.965535960161722,
0.000603907848525584));
#6954=CARTESIAN_POINT('Ctrl Pts',(0.687738022194911,-0.966226783953424,
0.12240713418347));
#6955=CARTESIAN_POINT('Ctrl Pts',(0.679740127500145,-0.944877535015784,
0.243976853099216));
#6956=CARTESIAN_POINT('Ctrl Pts',(0.671742232805379,-0.900384620032069,
0.356385477320749));
#6957=CARTESIAN_POINT('Ctrl Pts',(0.650526107584935,-0.782357652718426,
0.654573380307598));
#6958=CARTESIAN_POINT('Ctrl Pts',(0.629309982364491,-0.501471247814132,
0.888295665503207));
#6959=CARTESIAN_POINT('Ctrl Pts',(0.608093857144047,-0.186796400447701,
0.950160710409515));
#6960=CARTESIAN_POINT('Ctrl Pts',(0.586877731923603,0.127878446918726,1.01202575531582));
#6961=CARTESIAN_POINT('Ctrl Pts',(0.565661606703159,0.47634173674729,0.902033559932829));
#6962=CARTESIAN_POINT('Ctrl Pts',(0.544445481482716,0.698465791461622,0.670712394137428));
#6963=CARTESIAN_POINT('Ctrl Pts',(0.523229356262272,0.920589846175955,0.439391228342025));
#6964=CARTESIAN_POINT('Ctrl Pts',(0.502013231041828,1.01637466577606,0.0867410921342136));
#6965=CARTESIAN_POINT('Ctrl Pts',(0.480797105821384,0.941810253427243,-0.225160240747506));
#6966=CARTESIAN_POINT('Ctrl Pts',(0.45958098060094,0.867245841078429,-0.537061573629225));
#6967=CARTESIAN_POINT('Ctrl Pts',(0.438364855380496,0.622332196780702,-0.808214103184852));
#6968=CARTESIAN_POINT('Ctrl Pts',(0.417148730160052,0.319602326501539,-0.914072937871646));
#6969=CARTESIAN_POINT('Ctrl Pts',(0.395932604939608,0.0168724562223755,
-1.01993177255844));
#6970=CARTESIAN_POINT('Ctrl Pts',(0.374716479719165,-0.343673640038224,
-0.960496912376401));
#6971=CARTESIAN_POINT('Ctrl Pts',(0.353500354498721,-0.596341085022193,
-0.762976059833586));
#6972=CARTESIAN_POINT('Ctrl Pts',(0.334245541962373,-0.825650831107044,
-0.583714910673945));
#6973=CARTESIAN_POINT('Ctrl Pts',(0.314990729426024,-0.966105559516294,
-0.290718252710928));
#6974=CARTESIAN_POINT('Ctrl Pts',(0.295735916889676,-0.96799567585261,0.000586695936425057));
#6975=CARTESIAN_POINT('Ctrl Pts',(0.237764083110324,-0.96769285498825,0.00103535076607003));
#6976=CARTESIAN_POINT('Ctrl Pts',(0.256524972514437,-0.965508093804783,
-0.282730939306557));
#6977=CARTESIAN_POINT('Ctrl Pts',(0.275285861918551,-0.833247180307396,
-0.569078953342249));
#6978=CARTESIAN_POINT('Ctrl Pts',(0.294046751322664,-0.613997775944128,
-0.74904683801851));
#6979=CARTESIAN_POINT('Ctrl Pts',(0.315262876543107,-0.366055222833664,
-0.952567102687459));
#6980=CARTESIAN_POINT('Ctrl Pts',(0.336479001763551,-0.00686598179092317,
-1.02004135787579));
#6981=CARTESIAN_POINT('Ctrl Pts',(0.357695126983995,0.298275211789835,-0.921175933203103));
#6982=CARTESIAN_POINT('Ctrl Pts',(0.378911252204439,0.603416405370592,-0.822310508530412));
#6983=CARTESIAN_POINT('Ctrl Pts',(0.400127377424883,0.854509551489366,-0.557105403996695));
#6984=CARTESIAN_POINT('Ctrl Pts',(0.421343502645326,0.936297417272776,-0.247065280132184));
#6985=CARTESIAN_POINT('Ctrl Pts',(0.44255962786577,1.01808528305619,0.0629748437323275));
#6986=CARTESIAN_POINT('Ctrl Pts',(0.463775753086214,0.93056786850423,0.417849986927633));
#6987=CARTESIAN_POINT('Ctrl Pts',(0.484991878306658,0.713895687898178,0.654299743496954));
#6988=CARTESIAN_POINT('Ctrl Pts',(0.506208003527102,0.497223507292127,0.890749500066273));
#6989=CARTESIAN_POINT('Ctrl Pts',(0.527424128747546,0.151396560631982,1.00877387000961));
#6990=CARTESIAN_POINT('Ctrl Pts',(0.54864025396799,-0.16463713113037,0.954237787400182));
#6991=CARTESIAN_POINT('Ctrl Pts',(0.569856379188434,-0.480670822892721,
0.899701704790755));
#6992=CARTESIAN_POINT('Ctrl Pts',(0.591072504408878,-0.766911259757278,
0.672605169628564));
#6993=CARTESIAN_POINT('Ctrl Pts',(0.612288629629321,-0.891843900121912,
0.377250898045158));
#6994=CARTESIAN_POINT('Ctrl Pts',(0.620780447456322,-0.941848564574043,
0.259034463957746));
#6995=CARTESIAN_POINT('Ctrl Pts',(0.629272265283323,-0.966011322203064,
0.129882972155661));
#6996=CARTESIAN_POINT('Ctrl Pts',(0.637764083110324,-0.965403356746268,
0.000512007511799884));
#6997=CARTESIAN_POINT('Origin',(1.25,0.,0.));
#6998=CARTESIAN_POINT('',(1.09573591688968,-0.965800633193088,-0.00073910647511409));
#6999=CARTESIAN_POINT('',(1.03776408311032,-0.965986601461759,-0.000802905574952835));
#7000=CARTESIAN_POINT('',(1.25,-0.96675,-1.1839272930757E-16));
#7001=CARTESIAN_POINT('Ctrl Pts',(1.09573591688968,-0.965800633193088,-0.00073910647511409));
#7002=CARTESIAN_POINT('Ctrl Pts',(1.08170144018424,-0.964287961650603,0.212850295800185));
#7003=CARTESIAN_POINT('Ctrl Pts',(1.0676669634788,-0.894477007693264,0.427337796170151));
#7004=CARTESIAN_POINT('Ctrl Pts',(1.05363248677337,-0.764181677306994,0.594751173789774));
#7005=CARTESIAN_POINT('Ctrl Pts',(1.03241636155292,-0.567212306582722,0.847832443416278));
#7006=CARTESIAN_POINT('Ctrl Pts',(1.01120023633248,-0.232019113166176,0.993336094150022));
#7007=CARTESIAN_POINT('Ctrl Pts',(0.989984111112037,0.0873706532867941,
0.964400766431873));
#7008=CARTESIAN_POINT('Ctrl Pts',(0.968767985891593,0.406760419739764,0.935465438713724));
#7009=CARTESIAN_POINT('Ctrl Pts',(0.947551860671148,0.71034675922916,0.732091132543686));
#7010=CARTESIAN_POINT('Ctrl Pts',(0.926335735450704,0.858626252065649,0.447731661748216));
#7011=CARTESIAN_POINT('Ctrl Pts',(0.90511961023026,1.00690574490214,0.163372190952747));
#7012=CARTESIAN_POINT('Ctrl Pts',(0.883903485009817,0.999878391085719,-0.201972444468155));
#7013=CARTESIAN_POINT('Ctrl Pts',(0.862687359789374,0.840773489282268,-0.480419223503817));
#7014=CARTESIAN_POINT('Ctrl Pts',(0.84147123456893,0.681668587478818,-0.758866002539479));
#7015=CARTESIAN_POINT('Ctrl Pts',(0.820255109348486,0.370486137688336,-0.950414925189903));
#7016=CARTESIAN_POINT('Ctrl Pts',(0.799038984128042,0.0502198570115047,
-0.967046989745439));
#7017=CARTESIAN_POINT('Ctrl Pts',(0.777822858907598,-0.270046423665327,
-0.983679054300974));
#7018=CARTESIAN_POINT('Ctrl Pts',(0.756606733687153,-0.599396535228511,
-0.82539426076162));
#7019=CARTESIAN_POINT('Ctrl Pts',(0.73539060846671,-0.786487826148606,-0.564925103602899));
#7020=CARTESIAN_POINT('Ctrl Pts',(0.722172377941032,-0.903050854837064,
-0.402645642656119));
#7021=CARTESIAN_POINT('Ctrl Pts',(0.708954147415354,-0.96439422618299,-0.200701958996695));
#7022=CARTESIAN_POINT('Ctrl Pts',(0.695735916889677,-0.965535960161722,
0.000603907848525584));
#7023=CARTESIAN_POINT('Ctrl Pts',(0.637764083110324,-0.965403356746268,
0.000512007511799884));
#7024=CARTESIAN_POINT('Ctrl Pts',(0.650488390503767,-0.964492369309365,
-0.193339998672378));
#7025=CARTESIAN_POINT('Ctrl Pts',(0.66321269789721,-0.907964626205851,-0.387684778820973));
#7026=CARTESIAN_POINT('Ctrl Pts',(0.675937005290653,-0.79942395847086,-0.546471414702047));
#7027=CARTESIAN_POINT('Ctrl Pts',(0.697153130511097,-0.618446532590466,
-0.811227447861222));
#7028=CARTESIAN_POINT('Ctrl Pts',(0.71836925573154,-0.292866836964969,-0.977127506174948));
#7029=CARTESIAN_POINT('Ctrl Pts',(0.739585380951984,0.0277004179809616,
-0.967951999615512));
#7030=CARTESIAN_POINT('Ctrl Pts',(0.760801506172428,0.348267672926892,-0.958776493056076));
#7031=CARTESIAN_POINT('Ctrl Pts',(0.782017631392872,0.663822487193254,-0.774525421623477));
#7032=CARTESIAN_POINT('Ctrl Pts',(0.803233756613316,0.829364401714287,-0.49985784471143));
#7033=CARTESIAN_POINT('Ctrl Pts',(0.82444988183376,0.99490631623532,-0.225190267799384));
#7034=CARTESIAN_POINT('Ctrl Pts',(0.845666007054203,1.01043533101103,0.13989381459211));
#7035=CARTESIAN_POINT('Ctrl Pts',(0.866882132274647,0.868814199090254,0.427627717529623));
#7036=CARTESIAN_POINT('Ctrl Pts',(0.888098257495091,0.727193067169481,0.715361620467137));
#7037=CARTESIAN_POINT('Ctrl Pts',(0.909314382715535,0.428421788552229,0.925745343950671));
#7038=CARTESIAN_POINT('Ctrl Pts',(0.930530507935979,0.109791850608296,0.962105904569766));
#7039=CARTESIAN_POINT('Ctrl Pts',(0.951746633156423,-0.208838087335635,
0.99846646518886));
#7040=CARTESIAN_POINT('Ctrl Pts',(0.972962758376867,-0.547326684606245,
0.86080386294352));
#7041=CARTESIAN_POINT('Ctrl Pts',(0.99417888359731,-0.750132748216865,0.612375420712454));
#7042=CARTESIAN_POINT('Ctrl Pts',(1.00870728343498,-0.889010491019784,0.442256339010159));
#7043=CARTESIAN_POINT('Ctrl Pts',(1.02323568327265,-0.964263295846235,0.220196380992393));
#7044=CARTESIAN_POINT('Ctrl Pts',(1.03776408311032,-0.965986601461759,-0.000802905574952835));
#7045=CARTESIAN_POINT('Origin',(1.25,0.,0.));
#7046=CARTESIAN_POINT('',(1.49573591688968,-0.968224609176391,-0.00031821983524985));
#7047=CARTESIAN_POINT('',(1.43776408311032,-0.96830804582958,-0.000184094457921295));
#7048=CARTESIAN_POINT('',(1.25,-0.96675,-1.1839272930757E-16));
#7049=CARTESIAN_POINT('Ctrl Pts',(1.49573591688968,-0.968224609176391,-0.00031821983524985));
#7050=CARTESIAN_POINT('Ctrl Pts',(1.47566485817357,-0.966926994481933,0.3031765508298));
#7051=CARTESIAN_POINT('Ctrl Pts',(1.45559379945746,-0.812598430180798,0.607808692581674));
#7052=CARTESIAN_POINT('Ctrl Pts',(1.43552274074136,-0.566555587107941,0.785313598752052));
#7053=CARTESIAN_POINT('Ctrl Pts',(1.41430661552091,-0.306475845323378,0.972945271292166));
#7054=CARTESIAN_POINT('Ctrl Pts',(1.39309049030047,0.0560813988977043,1.01853056055889));
#7055=CARTESIAN_POINT('Ctrl Pts',(1.37187436508003,0.354514689861907,0.901122524422879));
#7056=CARTESIAN_POINT('Ctrl Pts',(1.35065823985958,0.65294798082611,0.783714488286868));
#7057=CARTESIAN_POINT('Ctrl Pts',(1.32944211463914,0.887257318533434,0.503313126748121));
#7058=CARTESIAN_POINT('Ctrl Pts',(1.30822598941869,0.949773311073654,0.188767720302581));
#7059=CARTESIAN_POINT('Ctrl Pts',(1.28700986419825,1.01228930361387,-0.125777686142959));
#7060=CARTESIAN_POINT('Ctrl Pts',(1.26579373897781,0.903011950986991,-0.474467137495291));
#7061=CARTESIAN_POINT('Ctrl Pts',(1.24457761375736,0.672156184097886,-0.697071481701902));
#7062=CARTESIAN_POINT('Ctrl Pts',(1.22336148853692,0.441300417208782,-0.919675825908513));
#7063=CARTESIAN_POINT('Ctrl Pts',(1.20214536331647,0.088866236057456,-1.0161950629694));
#7064=CARTESIAN_POINT('Ctrl Pts',(1.18092923809603,-0.223196554351772,-0.942276943640678));
#7065=CARTESIAN_POINT('Ctrl Pts',(1.15971311287559,-0.535259344761003,-0.868358824311952));
#7066=CARTESIAN_POINT('Ctrl Pts',(1.13849698765514,-0.806950744428136,-0.624003348593605));
#7067=CARTESIAN_POINT('Ctrl Pts',(1.1172808624347,-0.913423670245701,-0.321496166474798));
#7068=CARTESIAN_POINT('Ctrl Pts',(1.11009921391969,-0.949464706091843,-0.219097626087732));
#7069=CARTESIAN_POINT('Ctrl Pts',(1.10291756540468,-0.966574689509172,-0.110035950658669));
#7070=CARTESIAN_POINT('Ctrl Pts',(1.09573591688968,-0.965800633193088,-0.00073910647511409));
#7071=CARTESIAN_POINT('Ctrl Pts',(1.03776408311032,-0.965986601461759,-0.000802905574952835));
#7072=CARTESIAN_POINT('Ctrl Pts',(1.0444518084931,-0.966779874969921,-0.10253348532667));
#7073=CARTESIAN_POINT('Ctrl Pts',(1.05113953387587,-0.951992594196094,-0.204039313797799));
#7074=CARTESIAN_POINT('Ctrl Pts',(1.05782725925864,-0.92065867003448,-0.300150629635464));
#7075=CARTESIAN_POINT('Ctrl Pts',(1.07904338447909,-0.821254998290845,-0.605053955535511));
#7076=CARTESIAN_POINT('Ctrl Pts',(1.10025950969953,-0.55532412485295,-0.855666325118811));
#7077=CARTESIAN_POINT('Ctrl Pts',(1.12147563491997,-0.245066160482458,-0.936827173206812));
#7078=CARTESIAN_POINT('Ctrl Pts',(1.14269176014042,0.0651918038880355,-1.01798802129481));
#7079=CARTESIAN_POINT('Ctrl Pts',(1.16390788536086,0.419776859191126,-0.929697347887511));
#7080=CARTESIAN_POINT('Ctrl Pts',(1.1851240105813,0.655750876121149,-0.712526132007322));
#7081=CARTESIAN_POINT('Ctrl Pts',(1.20634013580175,0.891724893051173,-0.495354916127132));
#7082=CARTESIAN_POINT('Ctrl Pts',(1.22755626102219,1.00908787160813,-0.149303157774051));
#7083=CARTESIAN_POINT('Ctrl Pts',(1.24877238624264,0.953909384255206,0.166612060731162));
#7084=CARTESIAN_POINT('Ctrl Pts',(1.26998851146308,0.898730896902285,0.482527279236372));
#7085=CARTESIAN_POINT('Ctrl Pts',(1.29120463668352,0.671010943639489,0.768305957893716));
#7086=CARTESIAN_POINT('Ctrl Pts',(1.31242076190397,0.37539095120197,0.892627738781783));
#7087=CARTESIAN_POINT('Ctrl Pts',(1.33363688712441,0.079770958764452,1.01694951966985));
#7088=CARTESIAN_POINT('Ctrl Pts',(1.35485301234486,-0.283749072847788,0.979814402788641));
#7089=CARTESIAN_POINT('Ctrl Pts',(1.3760691375653,-0.548125202840523,0.798286573958416));
#7090=CARTESIAN_POINT('Ctrl Pts',(1.39663411941364,-0.804387374087343,0.622330009502189));
#7091=CARTESIAN_POINT('Ctrl Pts',(1.41719910126198,-0.967497900740498,0.310707828041999));
#7092=CARTESIAN_POINT('Ctrl Pts',(1.43776408311032,-0.96830804582958,-0.000184094457921295));
#7093=CARTESIAN_POINT('Origin',(1.25,0.,0.));
#7094=CARTESIAN_POINT('',(1.89573591688968,-0.966772019097869,0.00089209288056849));
#7095=CARTESIAN_POINT('',(1.83776408311032,-0.966544636178151,0.000891803094726289));
#7096=CARTESIAN_POINT('',(1.25,-0.96675,-1.1839272930757E-16));
#7097=CARTESIAN_POINT('Ctrl Pts',(1.89573591688968,-0.966772019097869,0.00089209288056849));
#7098=CARTESIAN_POINT('Ctrl Pts',(1.89084440138334,-0.967460921137827,0.0751428608741927));
#7099=CARTESIAN_POINT('Ctrl Pts',(1.88595288587701,-0.9596331226977,0.14925049718403));
#7100=CARTESIAN_POINT('Ctrl Pts',(1.88106137037068,-0.94274069279519,0.221232171309253));
#7101=CARTESIAN_POINT('Ctrl Pts',(1.85984524515023,-0.869472621248606,0.533440567631582));
#7102=CARTESIAN_POINT('Ctrl Pts',(1.83862911992979,-0.625676658048714,0.80565441474566));
#7103=CARTESIAN_POINT('Ctrl Pts',(1.81741299470935,-0.323389969041022,0.9127587334095));
#7104=CARTESIAN_POINT('Ctrl Pts',(1.7961968694889,-0.0211032800333296,1.01986305207334));
#7105=CARTESIAN_POINT('Ctrl Pts',(1.77498074426846,0.339674134782163,0.961857842286945));
#7106=CARTESIAN_POINT('Ctrl Pts',(1.75376461904802,0.59316308795535,0.765412190857585));
#7107=CARTESIAN_POINT('Ctrl Pts',(1.73254849382757,0.84665204112854,0.568966539428222));
#7108=CARTESIAN_POINT('Ctrl Pts',(1.71133236860713,0.992852532659421,0.234080446355895));
#7109=CARTESIAN_POINT('Ctrl Pts',(1.69011624338668,0.964580446894972,-0.0853676396729285));
#7110=CARTESIAN_POINT('Ctrl Pts',(1.66890011816624,0.936308361130523,-0.404815725701751));
#7111=CARTESIAN_POINT('Ctrl Pts',(1.6476839929458,0.733563698070743,-0.708825804687068));
#7112=CARTESIAN_POINT('Ctrl Pts',(1.62646786772535,0.449512511554961,-0.857695735862234));
#7113=CARTESIAN_POINT('Ctrl Pts',(1.60525174250491,0.16546132503918,-1.0065656670374));
#7114=CARTESIAN_POINT('Ctrl Pts',(1.58403561728446,-0.199896384932602,-1.00029545040241));
#7115=CARTESIAN_POINT('Ctrl Pts',(1.56281949206402,-0.478672858699194,-0.841768500692864));
#7116=CARTESIAN_POINT('Ctrl Pts',(1.54160336684358,-0.757449332465786,-0.683241550983313));
#7117=CARTESIAN_POINT('Ctrl Pts',(1.52038724162313,-0.949644570027188,-0.372457868199196));
#7118=CARTESIAN_POINT('Ctrl Pts',(1.49917111640269,-0.966941069133869,-0.0522269989003843));
#7119=CARTESIAN_POINT('Ctrl Pts',(1.49802604989835,-0.967874587463138,-0.0349436524703006));
#7120=CARTESIAN_POINT('Ctrl Pts',(1.49688098339401,-0.968298638909609,-0.0176327870957842));
#7121=CARTESIAN_POINT('Ctrl Pts',(1.49573591688968,-0.968224609176391,-0.00031821983524985));
#7122=CARTESIAN_POINT('Ctrl Pts',(1.43776408311032,-0.96830804582958,-0.000184094457921295));
#7123=CARTESIAN_POINT('Ctrl Pts',(1.43841522648243,-0.968333697231029,-0.0100277800137327));
#7124=CARTESIAN_POINT('Ctrl Pts',(1.43906636985453,-0.968196637926884,-0.0198707334643601));
#7125=CARTESIAN_POINT('Ctrl Pts',(1.43971751322663,-0.967894672944393,-0.0297086252262958));
#7126=CARTESIAN_POINT('Ctrl Pts',(1.46093363844708,-0.958055784682296,-0.350255454801532));
#7127=CARTESIAN_POINT('Ctrl Pts',(1.48214976366752,-0.773145779784875,-0.665428573172762));
#7128=CARTESIAN_POINT('Ctrl Pts',(1.50336588888796,-0.49813419844903,-0.83040044304409));
#7129=CARTESIAN_POINT('Ctrl Pts',(1.52458201410841,-0.223122617113181,-0.99537231291542));
#7130=CARTESIAN_POINT('Ctrl Pts',(1.54579813932885,0.141990540661093,-1.01014293428684));
#7131=CARTESIAN_POINT('Ctrl Pts',(1.56701426454929,0.429429381136857,-0.867924647533782));
#7132=CARTESIAN_POINT('Ctrl Pts',(1.58823038976974,0.716868221612619,-0.72570636078072));
#7133=CARTESIAN_POINT('Ctrl Pts',(1.60944651499018,0.926632744789872,-0.426499165903169));
#7134=CARTESIAN_POINT('Ctrl Pts',(1.63066264021063,0.962332115966355,-0.10779468641756));
#7135=CARTESIAN_POINT('Ctrl Pts',(1.65187876543107,0.998031487142837,0.210909793068051));
#7136=CARTESIAN_POINT('Ctrl Pts',(1.67309489065152,0.859665706318551,0.549111557161723));
#7137=CARTESIAN_POINT('Ctrl Pts',(1.69431101587196,0.610816854431274,0.751401884753216));
#7138=CARTESIAN_POINT('Ctrl Pts',(1.7155271410924,0.361968002543998,0.953692212344708));
#7139=CARTESIAN_POINT('Ctrl Pts',(1.73674326631284,0.00263607959373437,
1.02007110343402));
#7140=CARTESIAN_POINT('Ctrl Pts',(1.75795939153329,-0.302060451690969,0.920034271570729));
#7141=CARTESIAN_POINT('Ctrl Pts',(1.77917551675373,-0.606756982975677,0.819997439707436));
#7142=CARTESIAN_POINT('Ctrl Pts',(1.80039164197418,-0.856818122594822,0.553544884891533));
#7143=CARTESIAN_POINT('Ctrl Pts',(1.82160776719462,-0.937334401881812,0.243120124217056));
#7144=CARTESIAN_POINT('Ctrl Pts',(1.82699320583319,-0.95777241669368,0.164322818717865));
#7145=CARTESIAN_POINT('Ctrl Pts',(1.83237864447176,-0.967286105479931,0.0826922411753721));
#7146=CARTESIAN_POINT('Ctrl Pts',(1.83776408311032,-0.966544636178151,0.000891803094726289));
#7147=CARTESIAN_POINT('Origin',(1.25,0.,0.));
#7148=CARTESIAN_POINT('',(2.29573591688968,-0.964716333291436,0.000839189083712686));
#7149=CARTESIAN_POINT('',(2.23776408311032,-0.965144827742031,-0.000120440973035392));
#7150=CARTESIAN_POINT('',(1.25,-0.96675,-1.1839272930757E-16));
#7151=CARTESIAN_POINT('Ctrl Pts',(2.29573591688968,-0.964651808581398,0.000865815094782327));
#7152=CARTESIAN_POINT('Ctrl Pts',(2.28480781937267,-0.964804709789736,0.167104793299758));
#7153=CARTESIAN_POINT('Ctrl Pts',(2.27387972185567,-0.924102274326781,0.333140176983196));
#7154=CARTESIAN_POINT('Ctrl Pts',(2.26295162433867,-0.842840346924172,0.476636691321465));
#7155=CARTESIAN_POINT('Ctrl Pts',(2.24173549911822,-0.685076086059376,0.755224982848065));
#7156=CARTESIAN_POINT('Ctrl Pts',(2.22051937389778,-0.374437158674562,0.948860974182947));
#7157=CARTESIAN_POINT('Ctrl Pts',(2.19930324867734,-0.0541774433576252,
0.967020857490355));
#7158=CARTESIAN_POINT('Ctrl Pts',(2.17808712345689,0.266082271959314,0.985180740797765));
#7159=CARTESIAN_POINT('Ctrl Pts',(2.15687099823645,0.595962775208374,0.827864516077699));
#7160=CARTESIAN_POINT('Ctrl Pts',(2.135654873016,0.784103890128058,0.568079176717024));
#7161=CARTESIAN_POINT('Ctrl Pts',(2.11443874779556,0.97224500504774,0.308293837356353));
#7162=CARTESIAN_POINT('Ctrl Pts',(2.09322262257512,1.01864673163805,-0.0539606166449227));
#7163=CARTESIAN_POINT('Ctrl Pts',(2.07200649735467,0.901873588961803,-0.352587694431253));
#7164=CARTESIAN_POINT('Ctrl Pts',(2.05079037213423,0.785100446285557,-0.651214772217586));
#7165=CARTESIAN_POINT('Ctrl Pts',(2.02957424691379,0.505152434342748,-0.886214473788973));
#7166=CARTESIAN_POINT('Ctrl Pts',(2.00835812169334,0.190729503949967,-0.949408981360314));
#7167=CARTESIAN_POINT('Ctrl Pts',(1.9871419964729,-0.123693426442815,-1.01260348893165));
#7168=CARTESIAN_POINT('Ctrl Pts',(1.96592587125245,-0.472591275285571,-0.90399280250295));
#7169=CARTESIAN_POINT('Ctrl Pts',(1.94470974603201,-0.695670109760311,-0.673585986523306));
#7170=CARTESIAN_POINT('Ctrl Pts',(1.9283851363179,-0.867316669650043,-0.496300958873));
#7171=CARTESIAN_POINT('Ctrl Pts',(1.91206052660379,-0.964472924488232,-0.246907348192393));
#7172=CARTESIAN_POINT('Ctrl Pts',(1.89573591688968,-0.966772019097869,0.00089209288056849));
#7173=CARTESIAN_POINT('Ctrl Pts',(1.83776408311032,-0.966544636178151,0.000891803094726289));
#7174=CARTESIAN_POINT('Ctrl Pts',(1.8535947696922,-0.964365061047076,-0.239563466090049));
#7175=CARTESIAN_POINT('Ctrl Pts',(1.86942545627408,-0.873572025317322,-0.481486477651458));
#7176=CARTESIAN_POINT('Ctrl Pts',(1.88525614285595,-0.711162484222502,-0.657226222658887));
#7177=CARTESIAN_POINT('Ctrl Pts',(1.9064722680764,-0.493502868321361,-0.892750842327313));
#7178=CARTESIAN_POINT('Ctrl Pts',(1.92768839329684,-0.147212217564238,-1.00940311513113));
#7179=CARTESIAN_POINT('Ctrl Pts',(1.94890451851728,0.168589541409646,-0.953565539955677));
#7180=CARTESIAN_POINT('Ctrl Pts',(1.97012064373773,0.484391300383536,-0.897727964780228));
#7181=CARTESIAN_POINT('Ctrl Pts',(1.99133676895817,0.769704167574187,-0.669400541625513));
#7182=CARTESIAN_POINT('Ctrl Pts',(2.01255289417862,0.893408780830026,-0.373529828255184));
#7183=CARTESIAN_POINT('Ctrl Pts',(2.03376901939906,1.01711339408586,-0.0776591148848542));
#7184=CARTESIAN_POINT('Ctrl Pts',(2.0549851446195,0.979209753406891,0.285754888701089));
#7185=CARTESIAN_POINT('Ctrl Pts',(2.07620126983995,0.797139938097043,0.549766367596159));
#7186=CARTESIAN_POINT('Ctrl Pts',(2.09741739506039,0.615070122787196,0.813777846491227));
#7187=CARTESIAN_POINT('Ctrl Pts',(2.11863352028083,0.288834132846476,0.978386800695422));
#7188=CARTESIAN_POINT('Ctrl Pts',(2.13984964550128,-0.0317036593373814,
0.967858504908859));
#7189=CARTESIAN_POINT('Ctrl Pts',(2.16106577072172,-0.352241451521237,0.957330209122296));
#7190=CARTESIAN_POINT('Ctrl Pts',(2.18228189594217,-0.667081045948231,0.771664663344978));
#7191=CARTESIAN_POINT('Ctrl Pts',(2.20349802116261,-0.831458666207518,0.496357323535052));
#7192=CARTESIAN_POINT('Ctrl Pts',(2.21492004181185,-0.919953834546034,0.348141469437165));
#7193=CARTESIAN_POINT('Ctrl Pts',(2.22634206246109,-0.964839564100767,0.173944111700515));
#7194=CARTESIAN_POINT('Ctrl Pts',(2.23776408311032,-0.965144827742031,-0.000120440973035392));
#7195=CARTESIAN_POINT('Origin',(-0.572772559302386,0.,0.));
#7196=CARTESIAN_POINT('',(2.02722744069761,-0.739016831769666,0.000681930839134881));
#7197=CARTESIAN_POINT('',(2.10627255930239,-0.737772979261817,-9.20671105089643E-5));
#7198=CARTESIAN_POINT('',(-0.572772559302386,-0.739,-5.47916578054271E-15));
#7199=CARTESIAN_POINT('',(2.3266,0.00705397816592627,0.740208249496393));
#7200=CARTESIAN_POINT('Ctrl Pts',(2.02722744069761,-0.739016831769666,0.000681930839134901));
#7201=CARTESIAN_POINT('Ctrl Pts',(2.04355205041173,-0.737259365085908,-0.188740139968123));
#7202=CARTESIAN_POINT('Ctrl Pts',(2.08109278534628,-0.566469936104065,-0.627145185848076));
#7203=CARTESIAN_POINT('Ctrl Pts',(2.13984964550128,0.172150057567682,-0.857075020006521));
#7204=CARTESIAN_POINT('Ctrl Pts',(2.20349802116261,0.814140998842262,-0.318161817644216));
#7205=CARTESIAN_POINT('Ctrl Pts',(2.26574813932885,0.710067894618011,0.494328326954158));
#7206=CARTESIAN_POINT('Ctrl Pts',(2.30678213227465,0.23616540058745,0.736897610753465));
#7207=CARTESIAN_POINT('Ctrl Pts',(2.3266,0.00705185163866651,0.740219785066309));
#7208=CARTESIAN_POINT('',(2.3266,0.701646902936369,0.231975480600434));
#7209=CARTESIAN_POINT('Origin',(2.3266,0.,0.));
#7210=CARTESIAN_POINT('Ctrl Pts',(2.10627255930239,-0.737772979261817,-9.2067110508921E-5));
#7211=CARTESIAN_POINT('Ctrl Pts',(2.11606666387359,-0.737973070067811,-0.114185958198688));
#7212=CARTESIAN_POINT('Ctrl Pts',(2.14707689366524,-0.65927271946186,-0.475195283900803));
#7213=CARTESIAN_POINT('Ctrl Pts',(2.19930324867733,-0.0957849414937873,
-0.86944400077431));
#7214=CARTESIAN_POINT('Ctrl Pts',(2.26295162433867,0.68001209321599,-0.548823559975255));
#7215=CARTESIAN_POINT('Ctrl Pts',(2.30538387477956,0.778955542380413,-0.00185685071207135));
#7216=CARTESIAN_POINT('Ctrl Pts',(2.3266,0.701646902936369,0.231975480600434));
#7217=CARTESIAN_POINT('Origin',(-0.572772559302386,0.,0.));
#7218=CARTESIAN_POINT('',(1.62722744069761,-0.740127216117252,-0.000243252607449027));
#7219=CARTESIAN_POINT('',(1.70627255930239,-0.738843016432018,0.000681709321951329));
#7220=CARTESIAN_POINT('',(-0.572772559302386,-0.739,-5.47916578054271E-15));
#7221=CARTESIAN_POINT('Ctrl Pts',(1.62722744069761,-0.740127216117252,-0.000243252607449037));
#7222=CARTESIAN_POINT('Ctrl Pts',(1.62837250720195,-0.740183805693511,-0.013478799755662));
#7223=CARTESIAN_POINT('Ctrl Pts',(1.65073369892673,-0.73385366968859,-0.271891153010392));
#7224=CARTESIAN_POINT('Ctrl Pts',(1.69431101587196,-0.432089760676844,-0.759849648569051));
#7225=CARTESIAN_POINT('Ctrl Pts',(1.75795939153329,0.405767020298013,-0.774228826515532));
#7226=CARTESIAN_POINT('Ctrl Pts',(1.82160776719462,0.870711336826102,-0.0770575359952864));
#7227=CARTESIAN_POINT('Ctrl Pts',(1.88525614285595,0.535436974556678,0.690920191795093));
#7228=CARTESIAN_POINT('Ctrl Pts',(1.94890451851728,-0.291916041885991,0.823940672887867));
#7229=CARTESIAN_POINT('Ctrl Pts',(1.9962282844645,-0.707606442547758,0.359795648961634));
#7230=CARTESIAN_POINT('Ctrl Pts',(2.02233592519128,-0.739543440104323,0.0574404698071101));
#7231=CARTESIAN_POINT('Ctrl Pts',(2.02722744069761,-0.739016831769666,0.000681930839134901));
#7232=CARTESIAN_POINT('Ctrl Pts',(1.70627255930239,-0.738843016432019,0.000681709321951364));
#7233=CARTESIAN_POINT('Ctrl Pts',(1.72210324588426,-0.737176912452845,-0.18312635266672));
#7234=CARTESIAN_POINT('Ctrl Pts',(1.75915005768658,-0.574759015302088,-0.615897726532182));
#7235=CARTESIAN_POINT('Ctrl Pts',(1.81741299470935,0.152178910917555,-0.860775724524354));
#7236=CARTESIAN_POINT('Ctrl Pts',(1.88106137037068,0.806472809610774,-0.33716372852332));
#7237=CARTESIAN_POINT('Ctrl Pts',(1.94470974603201,0.71955026356962,0.496235646651272));
#7238=CARTESIAN_POINT('Ctrl Pts',(2.00835812169334,-0.0285906101811712,
0.873725226657167));
#7239=CARTESIAN_POINT('Ctrl Pts',(2.06221239278347,-0.639495616387645,0.513465547115104));
#7240=CARTESIAN_POINT('Ctrl Pts',(2.09485053865315,-0.737539630587503,0.132965811788644));
#7241=CARTESIAN_POINT('Ctrl Pts',(2.10627255930239,-0.737772979261817,-9.2067110508921E-5));
#7242=CARTESIAN_POINT('Origin',(-0.572772559302386,0.,0.));
#7243=CARTESIAN_POINT('',(1.22722744069761,-0.738274288005887,-0.000564985451368562));
#7244=CARTESIAN_POINT('',(1.30627255930239,-0.740190996501743,-0.000140724907590206));
#7245=CARTESIAN_POINT('',(-0.572772559302386,-0.739,-5.47916578054271E-15));
#7246=CARTESIAN_POINT('Ctrl Pts',(1.22722744069761,-0.738274288005887,-0.000564985451368596));
#7247=CARTESIAN_POINT('Ctrl Pts',(1.23440908921262,-0.738865989704968,-0.0841133359573396));
#7248=CARTESIAN_POINT('Ctrl Pts',(1.26280686294807,-0.687148195366904,-0.413770540317463));
#7249=CARTESIAN_POINT('Ctrl Pts',(1.31242076190396,-0.201475781147527,-0.850577571991093));
#7250=CARTESIAN_POINT('Ctrl Pts',(1.37606913756531,0.606744109840312,-0.629234775441834));
#7251=CARTESIAN_POINT('Ctrl Pts',(1.43971751322663,0.857344462334542,0.170397511755603));
#7252=CARTESIAN_POINT('Ctrl Pts',(1.50336588888797,0.32001443730518,0.813428097254852));
#7253=CARTESIAN_POINT('Ctrl Pts',(1.56586919804495,-0.496462244332193,0.710770306505323));
#7254=CARTESIAN_POINT('Ctrl Pts',(1.60715638198151,-0.739135297566226,0.231753267197539));
#7255=CARTESIAN_POINT('Ctrl Pts',(1.62722744069761,-0.740127216117252,-0.000243252607449037));
#7256=CARTESIAN_POINT('Ctrl Pts',(1.30627255930239,-0.740190996501743,-0.000140724907590199));
#7257=CARTESIAN_POINT('Ctrl Pts',(1.30692370267449,-0.740210604865509,-0.00766540411704673));
#7258=CARTESIAN_POINT('Ctrl Pts',(1.32879097126704,-0.736692111833655,-0.260346995818802));
#7259=CARTESIAN_POINT('Ctrl Pts',(1.37187436508003,-0.449657344341168,-0.749588466564275));
#7260=CARTESIAN_POINT('Ctrl Pts',(1.43552274074136,0.387638617164456,-0.783461202618526));
#7261=CARTESIAN_POINT('Ctrl Pts',(1.49917111640269,0.86868123199142,-0.0973041288729582));
#7262=CARTESIAN_POINT('Ctrl Pts',(1.56281949206402,0.551373824608492,0.678277263416331));
#7263=CARTESIAN_POINT('Ctrl Pts',(1.62646786772535,-0.272664316773187,0.830500694029215));
#7264=CARTESIAN_POINT('Ctrl Pts',(1.67428555680481,-0.703487412979108,0.371437303241661));
#7265=CARTESIAN_POINT('Ctrl Pts',(1.70088712066382,-0.739409808067928,0.0632113433965318));
#7266=CARTESIAN_POINT('Ctrl Pts',(1.70627255930239,-0.738843016432019,0.000681709321951364));
#7267=CARTESIAN_POINT('Origin',(-0.572772559302386,0.,0.));
#7268=CARTESIAN_POINT('',(0.827227440697613,-0.738071967478162,0.000461637341666832));
#7269=CARTESIAN_POINT('',(0.906272559302387,-0.738416445285999,-0.000613754558977386));
#7270=CARTESIAN_POINT('',(-0.572772559302386,-0.739,-5.47916578054271E-15));
#7271=CARTESIAN_POINT('Ctrl Pts',(0.827227440697613,-0.738071967478162,
0.000461637341666824));
#7272=CARTESIAN_POINT('Ctrl Pts',(0.840445671223291,-0.73719920677448,-0.153419961415631));
#7273=CARTESIAN_POINT('Ctrl Pts',(0.874880026969413,-0.61504271873664,-0.555561719131355));
#7274=CARTESIAN_POINT('Ctrl Pts',(0.93053050793598,0.0453327389257982,-0.872936419502457));
#7275=CARTESIAN_POINT('Ctrl Pts',(0.99417888359731,0.758952072968206,-0.433666741182324));
#7276=CARTESIAN_POINT('Ctrl Pts',(1.05782725925864,0.775067556196549,0.404160056571117));
#7277=CARTESIAN_POINT('Ctrl Pts',(1.12147563491997,0.0788680065218695,0.870548302528163));
#7278=CARTESIAN_POINT('Ctrl Pts',(1.1779423620663,-0.603081147802284,0.574521731828544));
#7279=CARTESIAN_POINT('Ctrl Pts',(1.21319296399218,-0.737117976374239,0.162706354896649));
#7280=CARTESIAN_POINT('Ctrl Pts',(1.22722744069761,-0.738274288005887,-0.000564985451368596));
#7281=CARTESIAN_POINT('Ctrl Pts',(0.906272559302387,-0.738416445285999,
-0.000613754558977378));
#7282=CARTESIAN_POINT('Ctrl Pts',(0.912960284685159,-0.739022836930718,
-0.0783783249613751));
#7283=CARTESIAN_POINT('Ctrl Pts',(0.940864135288376,-0.691859526234811,
-0.402126213356302));
#7284=CARTESIAN_POINT('Ctrl Pts',(0.989984111112038,-0.221217080729997,
-0.845658086769963));
#7285=CARTESIAN_POINT('Ctrl Pts',(1.05363248677337,0.591935303657854,-0.643185448607059));
#7286=CARTESIAN_POINT('Ctrl Pts',(1.1172808624347,0.861078022520812,0.15039794758511));
#7287=CARTESIAN_POINT('Ctrl Pts',(1.18092923809603,0.33885910720287,0.805760068695353));
#7288=CARTESIAN_POINT('Ctrl Pts',(1.24392647038526,-0.486254985425757,0.721471155828013));
#7289=CARTESIAN_POINT('Ctrl Pts',(1.28570757745405,-0.739571707936107,0.237510302480507));
#7290=CARTESIAN_POINT('Ctrl Pts',(1.30627255930239,-0.740190996501743,-0.000140724907590199));
#7291=CARTESIAN_POINT('Origin',(-0.572772559302386,0.,0.));
#7292=CARTESIAN_POINT('',(0.427227440697614,-0.739952215624597,0.000448480265853964));
#7293=CARTESIAN_POINT('',(0.506272559302387,-0.737970603191613,0.000391387174775056));
#7294=CARTESIAN_POINT('',(-0.572772559302386,-0.739,-5.47916578054271E-15));
#7295=CARTESIAN_POINT('Ctrl Pts',(0.427227440697614,-0.739952215624596,
0.000448480265853929));
#7296=CARTESIAN_POINT('Ctrl Pts',(0.446482253233962,-0.738507378828591,
-0.222229934060904));
#7297=CARTESIAN_POINT('Ctrl Pts',(0.486953190990754,-0.512839059320208,
-0.692987053973792));
#7298=CARTESIAN_POINT('Ctrl Pts',(0.54864025396799,0.288505105027068,-0.825086052852563));
#7299=CARTESIAN_POINT('Ctrl Pts',(0.612288629629321,0.850153462314954,-0.203265356679994));
#7300=CARTESIAN_POINT('Ctrl Pts',(0.675937005290653,0.630494869034967,0.605449773366773));
#7301=CARTESIAN_POINT('Ctrl Pts',(0.739585380951984,-0.168618773116491,
0.857689439427387));
#7302=CARTESIAN_POINT('Ctrl Pts',(0.790015526087638,-0.678988757841016,
0.433016557285913));
#7303=CARTESIAN_POINT('Ctrl Pts',(0.819229546002848,-0.738600044832254,
0.0935700772294608));
#7304=CARTESIAN_POINT('Ctrl Pts',(0.827227440697613,-0.738071967478162,
0.000461637341666824));
#7305=CARTESIAN_POINT('Ctrl Pts',(0.506272559302387,-0.737970603191613,
0.000391387174775012));
#7306=CARTESIAN_POINT('Ctrl Pts',(0.51899686669583,-0.737274229035035,-0.147792354816542));
#7307=CARTESIAN_POINT('Ctrl Pts',(0.552937299309717,-0.622015155205619,
-0.544057942892273));
#7308=CARTESIAN_POINT('Ctrl Pts',(0.608093857144047,0.0250062607190412,
-0.873749542443373));
#7309=CARTESIAN_POINT('Ctrl Pts',(0.671742232805379,0.748652522139804,-0.451215665674743));
#7310=CARTESIAN_POINT('Ctrl Pts',(0.73539060846671,0.784264444309691,0.386013618692408));
#7311=CARTESIAN_POINT('Ctrl Pts',(0.799038984128041,0.0991070357816886,
0.868476214982029));
#7312=CARTESIAN_POINT('Ctrl Pts',(0.855999634406602,-0.595570363064826,
0.585952374541452));
#7313=CARTESIAN_POINT('Ctrl Pts',(0.891744159464716,-0.7370991214175,0.16832182627709));
#7314=CARTESIAN_POINT('Ctrl Pts',(0.906272559302387,-0.738416445285999,
-0.000613754558977378));
#7315=CARTESIAN_POINT('Origin',(2.3266,2.39206768658147E-16,-5.43753587379397E-17));
#7316=CARTESIAN_POINT('',(2.3266,-0.855344277194458,-0.450546035351206));
#7317=CARTESIAN_POINT('Ctrl Pts',(2.3266,0.00705185163866655,0.740219785066309));
#7318=CARTESIAN_POINT('Ctrl Pts',(2.3266,-0.0091816416561815,0.742895096882004));
#7319=CARTESIAN_POINT('Ctrl Pts',(2.3266,-0.0254819710138712,0.744984144680738));
#7320=CARTESIAN_POINT('Ctrl Pts',(2.3266,-0.0418213189100594,0.746474642718444));
#7321=CARTESIAN_POINT('Ctrl Pts',(2.3266,-0.0752275148083482,0.749522002365228));
#7322=CARTESIAN_POINT('Ctrl Pts',(2.3266,-0.108795641758076,0.75007069080123));
#7323=CARTESIAN_POINT('Ctrl Pts',(2.3266,-0.142321448506824,0.748288394145316));
#7324=CARTESIAN_POINT('Ctrl Pts',(2.3266,-0.159005045099053,0.747401461919111));
#7325=CARTESIAN_POINT('Ctrl Pts',(2.3266,-0.175678490901637,0.745936553914972));
#7326=CARTESIAN_POINT('Ctrl Pts',(2.3266,-0.192318008684797,0.74391008090649));
#7327=CARTESIAN_POINT('Ctrl Pts',(2.3266,-0.20132065718867,0.74281367748689));
#7328=CARTESIAN_POINT('Ctrl Pts',(2.3266,-0.210304455697944,0.741553895478701));
#7329=CARTESIAN_POINT('Ctrl Pts',(2.3266,-0.219262804535322,0.740134541391542));
#7330=CARTESIAN_POINT('Ctrl Pts',(2.3266,-0.254598126832081,0.734536039364728));
#7331=CARTESIAN_POINT('Ctrl Pts',(2.3266,-0.289549801717428,0.72645730926244));
#7332=CARTESIAN_POINT('Ctrl Pts',(2.3266,-0.323887860257361,0.716079004587159));
#7333=CARTESIAN_POINT('Ctrl Pts',(2.3266,-0.338421060949871,0.711686502765355));
#7334=CARTESIAN_POINT('Ctrl Pts',(2.3266,-0.352844521793266,0.706881436906426));
#7335=CARTESIAN_POINT('Ctrl Pts',(2.3266,-0.36714126863909,0.701674762529288));
#7336=CARTESIAN_POINT('Ctrl Pts',(2.3266,-0.376760163394388,0.698171696174481));
#7337=CARTESIAN_POINT('Ctrl Pts',(2.3266,-0.386321702824635,0.694486802926217));
#7338=CARTESIAN_POINT('Ctrl Pts',(2.3266,-0.395820709108693,0.690623021799272));
#7339=CARTESIAN_POINT('Ctrl Pts',(2.3266,-0.403344093306561,0.687562837501546));
#7340=CARTESIAN_POINT('Ctrl Pts',(2.3266,-0.410819442882381,0.684394007476334));
#7341=CARTESIAN_POINT('Ctrl Pts',(2.3266,-0.418243797843197,0.681118946191534));
#7342=CARTESIAN_POINT('Ctrl Pts',(2.3266,-0.452853461534587,0.665851792313006));
#7343=CARTESIAN_POINT('Ctrl Pts',(2.3266,-0.486357659396555,0.648279158997269));
#7344=CARTESIAN_POINT('Ctrl Pts',(2.3266,-0.518509938036373,0.628592801474918));
#7345=CARTESIAN_POINT('Ctrl Pts',(2.3266,-0.550872267895178,0.608777832744591));
#7346=CARTESIAN_POINT('Ctrl Pts',(2.3266,-0.58186630614572,0.586821105901194));
#7347=CARTESIAN_POINT('Ctrl Pts',(2.3266,-0.611237088993447,0.562865246568347));
#7348=CARTESIAN_POINT('Ctrl Pts',(2.3266,-0.626354028635055,0.550535330764774));
#7349=CARTESIAN_POINT('Ctrl Pts',(2.3266,-0.641040769620426,0.53767500060788));
#7350=CARTESIAN_POINT('Ctrl Pts',(2.3266,-0.6552603442492,0.524298749950964));
#7351=CARTESIAN_POINT('Ctrl Pts',(2.3266,-0.660929329845617,0.518965976342203));
#7352=CARTESIAN_POINT('Ctrl Pts',(2.3266,-0.666523772205263,0.513551232266967));
#7353=CARTESIAN_POINT('Ctrl Pts',(2.3266,-0.67203149961292,0.508065585358026));
#7354=CARTESIAN_POINT('Ctrl Pts',(2.3266,-0.699029329476628,0.481175989890019));
#7355=CARTESIAN_POINT('Ctrl Pts',(2.3266,-0.72400691357688,0.452528609055507));
#7356=CARTESIAN_POINT('Ctrl Pts',(2.3266,-0.746728020736309,0.422283976342188));
#7357=CARTESIAN_POINT('Ctrl Pts',(2.3266,-0.769504982910754,0.391964993624598));
#7358=CARTESIAN_POINT('Ctrl Pts',(2.3266,-0.790016116737887,0.360040749577662));
#7359=CARTESIAN_POINT('Ctrl Pts',(2.3266,-0.808289814214594,0.326779688833403));
#7360=CARTESIAN_POINT('Ctrl Pts',(2.3266,-0.81696709711708,0.310985642002837));
#7361=CARTESIAN_POINT('Ctrl Pts',(2.3266,-0.825139367604472,0.294889551675988));
#7362=CARTESIAN_POINT('Ctrl Pts',(2.3266,-0.832806738358023,0.278517287953485));
#7363=CARTESIAN_POINT('Ctrl Pts',(2.3266,-0.837430380466189,0.268644348403992));
#7364=CARTESIAN_POINT('Ctrl Pts',(2.3266,-0.841870381472551,0.258670948237785));
#7365=CARTESIAN_POINT('Ctrl Pts',(2.3266,-0.846126407283495,0.248602508196632));
#7366=CARTESIAN_POINT('Ctrl Pts',(2.3266,-0.849263221090139,0.241181777417403));
#7367=CARTESIAN_POINT('Ctrl Pts',(2.3266,-0.852296360098048,0.233718192729926));
#7368=CARTESIAN_POINT('Ctrl Pts',(2.3266,-0.855225532626083,0.226216366154033));
#7369=CARTESIAN_POINT('Ctrl Pts',(2.3266,-0.869632326082018,0.189319507062694));
#7370=CARTESIAN_POINT('Ctrl Pts',(2.3266,-0.881533437703762,0.151485642669957));
#7371=CARTESIAN_POINT('Ctrl Pts',(2.3266,-0.890969066035468,0.113010070419481));
#7372=CARTESIAN_POINT('Ctrl Pts',(2.3266,-0.900622821965197,0.0736450413291914));
#7373=CARTESIAN_POINT('Ctrl Pts',(2.3266,-0.907696290859194,0.0336073077901501));
#7374=CARTESIAN_POINT('Ctrl Pts',(2.3266,-0.912190086870429,-0.00682105459462326));
#7375=CARTESIAN_POINT('Ctrl Pts',(2.3266,-0.914349459355949,-0.0262478138756487));
#7376=CARTESIAN_POINT('Ctrl Pts',(2.3266,-0.915912511260161,-0.0457651761268934));
#7377=CARTESIAN_POINT('Ctrl Pts',(2.3266,-0.916875413994828,-0.0653434748872564));
#7378=CARTESIAN_POINT('Ctrl Pts',(2.3266,-0.917299664358875,-0.0739695801806303));
#7379=CARTESIAN_POINT('Ctrl Pts',(2.3266,-0.917607376849151,-0.0826075237982675));
#7380=CARTESIAN_POINT('Ctrl Pts',(2.3266,-0.917798058061557,-0.0912548003913321));
#7381=CARTESIAN_POINT('Ctrl Pts',(2.3266,-0.917979847998161,-0.09949886305392));
#7382=CARTESIAN_POINT('Ctrl Pts',(2.3266,-0.918055035202284,-0.107741728314853));
#7383=CARTESIAN_POINT('Ctrl Pts',(2.3266,-0.918023912658678,-0.115979255927813));
#7384=CARTESIAN_POINT('Ctrl Pts',(2.3266,-0.917864023310433,-0.15829883423272));
#7385=CARTESIAN_POINT('Ctrl Pts',(2.3266,-0.91490237027171,-0.200490667473989));
#7386=CARTESIAN_POINT('Ctrl Pts',(2.3266,-0.909156732986574,-0.242248418365806));
#7387=CARTESIAN_POINT('Ctrl Pts',(2.3266,-0.903451049303708,-0.283715797191301));
#7388=CARTESIAN_POINT('Ctrl Pts',(2.3266,-0.895000225390717,-0.324756379279632));
#7389=CARTESIAN_POINT('Ctrl Pts',(2.3266,-0.883773539295331,-0.365084529739219));
#7390=CARTESIAN_POINT('Ctrl Pts',(2.3266,-0.875731688688448,-0.39397221382448));
#7391=CARTESIAN_POINT('Ctrl Pts',(2.3266,-0.866264537064502,-0.422494697859053));
#7392=CARTESIAN_POINT('Ctrl Pts',(2.3266,-0.855344277194458,-0.450546035351206));
#7393=CARTESIAN_POINT('',(2.3266,-0.96675,-1.1839272930757E-16));
#7394=CARTESIAN_POINT('Origin',(2.3266,0.,0.));
#7395=CARTESIAN_POINT('',(2.3266,-0.168638537403571,-0.953577585643768));
#7396=CARTESIAN_POINT('Origin',(2.3266,0.,0.));
#7397=CARTESIAN_POINT('Ctrl Pts',(2.3266,-0.16863827771112,-0.953592946438969));
#7398=CARTESIAN_POINT('Ctrl Pts',(2.3266,-0.147465654530663,-0.954986799957863));
#7399=CARTESIAN_POINT('Ctrl Pts',(2.3266,-0.126272781527092,-0.955629173556653));
#7400=CARTESIAN_POINT('Ctrl Pts',(2.3266,-0.10508809158694,-0.955496709949245));
#7401=CARTESIAN_POINT('Ctrl Pts',(2.3266,-0.0672410987773937,-0.955260060311641));
#7402=CARTESIAN_POINT('Ctrl Pts',(2.3266,-0.0294193568307657,-0.952552042729772));
#7403=CARTESIAN_POINT('Ctrl Pts',(2.3266,0.00817672626721474,-0.947478640546724));
#7404=CARTESIAN_POINT('Ctrl Pts',(2.3266,0.029679781676428,-0.944576911449813));
#7405=CARTESIAN_POINT('Ctrl Pts',(2.3266,0.0511088134843331,-0.940900810877595));
#7406=CARTESIAN_POINT('Ctrl Pts',(2.3266,0.0724238415269682,-0.936466009340783));
#7407=CARTESIAN_POINT('Ctrl Pts',(2.3266,0.0839551864399211,-0.934066799448158));
#7408=CARTESIAN_POINT('Ctrl Pts',(2.3266,0.0954546673735591,-0.931444891816811));
#7409=CARTESIAN_POINT('Ctrl Pts',(2.3266,0.106895029296963,-0.928608210414757));
#7410=CARTESIAN_POINT('Ctrl Pts',(2.3266,0.147435171064247,-0.918556127538547));
#7411=CARTESIAN_POINT('Ctrl Pts',(2.3266,0.187295630759207,-0.905798999992378));
#7412=CARTESIAN_POINT('Ctrl Pts',(2.3266,0.226199649503474,-0.890473975822821));
#7413=CARTESIAN_POINT('Ctrl Pts',(2.3266,0.248473621616919,-0.881699839576527));
#7414=CARTESIAN_POINT('Ctrl Pts',(2.3266,0.270433587385743,-0.872083121950981));
#7415=CARTESIAN_POINT('Ctrl Pts',(2.3266,0.292022276599161,-0.861643953482181));
#7416=CARTESIAN_POINT('Ctrl Pts',(2.3266,0.300263240856417,-0.857659051324555));
#7417=CARTESIAN_POINT('Ctrl Pts',(2.3266,0.308450056697937,-0.853554269336753));
#7418=CARTESIAN_POINT('Ctrl Pts',(2.3266,0.31657934911869,-0.849330600533629));
#7419=CARTESIAN_POINT('Ctrl Pts',(2.3266,0.323957422231335,-0.845497236494036));
#7420=CARTESIAN_POINT('Ctrl Pts',(2.3266,0.331284238554771,-0.84156787828759));
#7421=CARTESIAN_POINT('Ctrl Pts',(2.3266,0.338550765117836,-0.837547399129169));
#7422=CARTESIAN_POINT('Ctrl Pts',(2.3266,0.373670084967107,-0.818116314375472));
#7423=CARTESIAN_POINT('Ctrl Pts',(2.3266,0.407433256551024,-0.796534237223156));
#7424=CARTESIAN_POINT('Ctrl Pts',(2.3266,0.439589982929631,-0.772920787990529));
#7425=CARTESIAN_POINT('Ctrl Pts',(2.3266,0.470995194774116,-0.749859193759874));
#7426=CARTESIAN_POINT('Ctrl Pts',(2.3266,0.500868881519513,-0.724859244899778));
#7427=CARTESIAN_POINT('Ctrl Pts',(2.3266,0.528937790278082,-0.698005501260112));
#7428=CARTESIAN_POINT('Ctrl Pts',(2.3266,0.541876813655034,-0.685626636812585));
#7429=CARTESIAN_POINT('Ctrl Pts',(2.3266,0.554431696369729,-0.672853541668634));
#7430=CARTESIAN_POINT('Ctrl Pts',(2.3266,0.566572088464898,-0.659693216914725));
#7431=CARTESIAN_POINT('Ctrl Pts',(2.3266,0.572732958972858,-0.653014762379159));
#7432=CARTESIAN_POINT('Ctrl Pts',(2.3266,0.578787048944214,-0.646236576282453));
#7433=CARTESIAN_POINT('Ctrl Pts',(2.3266,0.584730139804016,-0.639359518753095));
#7434=CARTESIAN_POINT('Ctrl Pts',(2.3266,0.589432586433977,-0.633918074769507));
#7435=CARTESIAN_POINT('Ctrl Pts',(2.3266,0.594063483497632,-0.628416996597973));
#7436=CARTESIAN_POINT('Ctrl Pts',(2.3266,0.598615889829617,-0.622863232110901));
#7437=CARTESIAN_POINT('Ctrl Pts',(2.3266,0.621523554501612,-0.594916742878777));
#7438=CARTESIAN_POINT('Ctrl Pts',(2.3266,0.642487414808634,-0.565591201764512));
#7439=CARTESIAN_POINT('Ctrl Pts',(2.3266,0.661292448179919,-0.534963557358698));
#7440=CARTESIAN_POINT('Ctrl Pts',(2.3266,0.678661125771888,-0.506675296945486));
#7441=CARTESIAN_POINT('Ctrl Pts',(2.3266,0.69418763594692,-0.477275294544982));
#7442=CARTESIAN_POINT('Ctrl Pts',(2.3266,0.707850085022545,-0.446949904939736));
#7443=CARTESIAN_POINT('Ctrl Pts',(2.3266,0.721108132135827,-0.417522132372059));
#7444=CARTESIAN_POINT('Ctrl Pts',(2.3266,0.732610655706484,-0.387222336042198));
#7445=CARTESIAN_POINT('Ctrl Pts',(2.3266,0.742311682314211,-0.356223725233837));
#7446=CARTESIAN_POINT('Ctrl Pts',(2.3266,0.74472416850348,-0.348514879202826));
#7447=CARTESIAN_POINT('Ctrl Pts',(2.3266,0.747022672915413,-0.340770513432795));
#7448=CARTESIAN_POINT('Ctrl Pts',(2.3266,0.749205684083773,-0.332998578461517));
#7449=CARTESIAN_POINT('Ctrl Pts',(2.3266,0.759292423406657,-0.297087867959487));
#7450=CARTESIAN_POINT('Ctrl Pts',(2.3266,0.766928667050838,-0.260553256960538));
#7451=CARTESIAN_POINT('Ctrl Pts',(2.3266,0.772094075526193,-0.223665502925765));
#7452=CARTESIAN_POINT('Ctrl Pts',(2.3266,0.777195092102294,-0.187237591041495));
#7453=CARTESIAN_POINT('Ctrl Pts',(2.3266,0.779886220465533,-0.15046400931105));
#7454=CARTESIAN_POINT('Ctrl Pts',(2.3266,0.780099171435814,-0.113617901149199));
#7455=CARTESIAN_POINT('Ctrl Pts',(2.3266,0.780199873465589,-0.0961938064089577));
#7456=CARTESIAN_POINT('Ctrl Pts',(2.3266,0.779745712369878,-0.0787537915307566));
#7457=CARTESIAN_POINT('Ctrl Pts',(2.3266,0.778725867603093,-0.0613289396111699));
#7458=CARTESIAN_POINT('Ctrl Pts',(2.3266,0.778171162891524,-0.0518513722666234));
#7459=CARTESIAN_POINT('Ctrl Pts',(2.3266,0.777448585933176,-0.0423751470953692));
#7460=CARTESIAN_POINT('Ctrl Pts',(2.3266,0.77655899786828,-0.0329302576238707));
#7461=CARTESIAN_POINT('Ctrl Pts',(2.3266,0.7732468432591,0.00223538300316667));
#7462=CARTESIAN_POINT('Ctrl Pts',(2.3266,0.767620707505793,0.0370380579314474));
#7463=CARTESIAN_POINT('Ctrl Pts',(2.3266,0.759636976250263,0.0712350618987401));
#7464=CARTESIAN_POINT('Ctrl Pts',(2.3266,0.751943629281566,0.104188252379458));
#7465=CARTESIAN_POINT('Ctrl Pts',(2.3266,0.742060610076505,0.136579845357312));
#7466=CARTESIAN_POINT('Ctrl Pts',(2.3266,0.729909685892531,0.168165888140475));
#7467=CARTESIAN_POINT('Ctrl Pts',(2.3266,0.721569647399475,0.189845622839368));
#7468=CARTESIAN_POINT('Ctrl Pts',(2.3266,0.712160386241925,0.211145303211162));
#7469=CARTESIAN_POINT('Ctrl Pts',(2.3266,0.70164690293637,0.231975480600428));
#7470=CARTESIAN_POINT('Ctrl Pts',(0.0352584761920629,-0.324968229607101,
0.663714283216827));
#7471=CARTESIAN_POINT('Ctrl Pts',(0.0564746014125068,-0.546159055819686,
0.555414683498625));
#7472=CARTESIAN_POINT('Ctrl Pts',(0.0989068518533947,-0.867866968611021,
0.10213065993041));
#7473=CARTESIAN_POINT('Ctrl Pts',(0.162555227514726,-0.554389096255145,
-0.676579895838483));
#7474=CARTESIAN_POINT('Ctrl Pts',(0.226203603176058,0.269321839759082,-0.831315270808783));
#7475=CARTESIAN_POINT('Ctrl Pts',(0.289851978837389,0.845141343193606,-0.223133510528201));
#7476=CARTESIAN_POINT('Ctrl Pts',(0.35350035449872,0.644441981350638,0.590684118087253));
#7477=CARTESIAN_POINT('Ctrl Pts',(0.417148730160053,-0.148625865295904,
0.86134357313186));
#7478=CARTESIAN_POINT('Ctrl Pts',(0.480797105821384,-0.805046913683514,
0.340554311735867));
#7479=CARTESIAN_POINT('Ctrl Pts',(0.544445481482716,-0.721629565711504,
-0.493299137187071));
#7480=CARTESIAN_POINT('Ctrl Pts',(0.608093857144047,0.0250062607190412,
-0.873749542443373));
#7481=CARTESIAN_POINT('Ctrl Pts',(0.671742232805379,0.748652522139804,-0.451215665674743));
#7482=CARTESIAN_POINT('Ctrl Pts',(0.73539060846671,0.784264444309691,0.386013618692408));
#7483=CARTESIAN_POINT('Ctrl Pts',(0.799038984128041,0.0991070357816886,
0.868476214982029));
#7484=CARTESIAN_POINT('Ctrl Pts',(0.862687359789374,-0.677132136857513,
0.552781372284408));
#7485=CARTESIAN_POINT('Ctrl Pts',(0.926335735450704,-0.831063210972372,
-0.270941124405154));
#7486=CARTESIAN_POINT('Ctrl Pts',(0.989984111112038,-0.221217080729997,
-0.845658086769963));
#7487=CARTESIAN_POINT('Ctrl Pts',(1.05363248677337,0.591935303657854,-0.643185448607059));
#7488=CARTESIAN_POINT('Ctrl Pts',(1.1172808624347,0.861078022520812,0.15039794758511));
#7489=CARTESIAN_POINT('Ctrl Pts',(1.18092923809603,0.33885910720287,0.805760068695353));
#7490=CARTESIAN_POINT('Ctrl Pts',(1.24457761375736,-0.494783416804721,0.720599940300586));
#7491=CARTESIAN_POINT('Ctrl Pts',(1.30822598941869,-0.873702320661405,-0.0268175294771084));
#7492=CARTESIAN_POINT('Ctrl Pts',(1.37187436508003,-0.449657344341168,-0.749588466564275));
#7493=CARTESIAN_POINT('Ctrl Pts',(1.43552274074136,0.387638617164456,-0.783461202618526));
#7494=CARTESIAN_POINT('Ctrl Pts',(1.49917111640269,0.86868123199142,-0.0973041288729582));
#7495=CARTESIAN_POINT('Ctrl Pts',(1.56281949206402,0.551373824608492,0.678277263416331));
#7496=CARTESIAN_POINT('Ctrl Pts',(1.62646786772535,-0.272664316773187,0.830500694029215));
#7497=CARTESIAN_POINT('Ctrl Pts',(1.69011624338669,-0.846117170701959,0.219458217663196));
#7498=CARTESIAN_POINT('Ctrl Pts',(1.75376461904801,-0.64195232541919,-0.593262832043307));
#7499=CARTESIAN_POINT('Ctrl Pts',(1.81741299470935,0.152178910917555,-0.860775724524354));
#7500=CARTESIAN_POINT('Ctrl Pts',(1.88106137037068,0.806472809610774,-0.33716372852332));
#7501=CARTESIAN_POINT('Ctrl Pts',(1.94470974603201,0.71955026356962,0.496235646651272));
#7502=CARTESIAN_POINT('Ctrl Pts',(2.00835812169334,-0.0285906101811712,
0.873725226657167));
#7503=CARTESIAN_POINT('Ctrl Pts',(2.07200649735467,-0.750596693289163,0.447947605774497));
#7504=CARTESIAN_POINT('Ctrl Pts',(2.13565487301601,-0.782508756785437,-0.388972207754245));
#7505=CARTESIAN_POINT('Ctrl Pts',(2.19930324867733,-0.0957849414937873,
-0.86944400077431));
#7506=CARTESIAN_POINT('Ctrl Pts',(2.26295162433867,0.68001209321599,-0.548823559975255));
#7507=CARTESIAN_POINT('Ctrl Pts',(2.30538387477956,0.778955542380413,-0.00185685071207135));
#7508=CARTESIAN_POINT('Ctrl Pts',(2.3266,0.701646902936369,0.231975480600434));
#7509=CARTESIAN_POINT('Ctrl Pts',(0.079088984128042,-0.358351862576436,
0.731896930038042));
#7510=CARTESIAN_POINT('Ctrl Pts',(0.100305109348486,-0.60226538191934,0.612471830168365));
#7511=CARTESIAN_POINT('Ctrl Pts',(0.142737359789373,-0.95702199887767,0.11262243160346));
#7512=CARTESIAN_POINT('Ctrl Pts',(0.206385735450706,-0.611340885462232,
-0.746084213058696));
#7513=CARTESIAN_POINT('Ctrl Pts',(0.270034111112036,0.296988979589994,-0.916715384893899));
#7514=CARTESIAN_POINT('Ctrl Pts',(0.333682486773368,0.931961794665117,-0.246055773506459));
#7515=CARTESIAN_POINT('Ctrl Pts',(0.3973308624347,0.710644805551184,0.651364455432481));
#7516=CARTESIAN_POINT('Ctrl Pts',(0.460979238096031,-0.163894038873325,
0.949828462072222));
#7517=CARTESIAN_POINT('Ctrl Pts',(0.524627613757363,-0.887748507996287,
0.375539085979369));
#7518=CARTESIAN_POINT('Ctrl Pts',(0.588275989418695,-0.795761786546325,
-0.543975221307212));
#7519=CARTESIAN_POINT('Ctrl Pts',(0.651924365080026,0.027575126699538,-0.963508883125141));
#7520=CARTESIAN_POINT('Ctrl Pts',(0.715572740741357,0.825560781913074,-0.497568560513454));
#7521=CARTESIAN_POINT('Ctrl Pts',(0.779221116402689,0.864831078135372,0.425668378122807));
#7522=CARTESIAN_POINT('Ctrl Pts',(0.842869492064021,0.109288193832785,0.957693832466087));
#7523=CARTESIAN_POINT('Ctrl Pts',(0.906517867725353,-0.746693185197295,
0.609568001755664));
#7524=CARTESIAN_POINT('Ctrl Pts',(0.970166243386683,-0.916437431224496,
-0.298774611587505));
#7525=CARTESIAN_POINT('Ctrl Pts',(1.03381461904802,-0.24394247095835,-0.932531622747347));
#7526=CARTESIAN_POINT('Ctrl Pts',(1.09746299470935,0.652744173936643,-0.709259190564775));
#7527=CARTESIAN_POINT('Ctrl Pts',(1.16111137037068,0.949535631735567,0.165848165249749));
#7528=CARTESIAN_POINT('Ctrl Pts',(1.22475974603201,0.373669734927479,0.888534924647256));
#7529=CARTESIAN_POINT('Ctrl Pts',(1.28840812169334,-0.545611979356493,0.794626388836201));
#7530=CARTESIAN_POINT('Ctrl Pts',(1.35205649735467,-0.963456810300842,-0.0295724651281722));
#7531=CARTESIAN_POINT('Ctrl Pts',(1.415704873016,-0.495850154523263,-0.826592874890849));
#7532=CARTESIAN_POINT('Ctrl Pts',(1.47935324867734,0.427460310921427,-0.86394532029844));
#7533=CARTESIAN_POINT('Ctrl Pts',(1.54300162433867,0.957919910649988,-0.107300076257179));
#7534=CARTESIAN_POINT('Ctrl Pts',(1.60665,0.608015858237083,0.747955949362685));
#7535=CARTESIAN_POINT('Ctrl Pts',(1.67029837566133,-0.300674825634303,0.915817127527255));
#7536=CARTESIAN_POINT('Ctrl Pts',(1.73394675132266,-0.933037867872626,0.242002921800675));
#7537=CARTESIAN_POINT('Ctrl Pts',(1.79759512698399,-0.70789938997229,-0.654208077870038));
#7538=CARTESIAN_POINT('Ctrl Pts',(1.86124350264533,0.167812085009332,-0.949202278994549));
#7539=CARTESIAN_POINT('Ctrl Pts',(1.92489187830666,0.88932088466213,-0.371800191839147));
#7540=CARTESIAN_POINT('Ctrl Pts',(1.98854025396799,0.793468879955719,0.547213395196526));
#7541=CARTESIAN_POINT('Ctrl Pts',(2.05218862962932,-0.0315276924855277,
0.963482069404649));
#7542=CARTESIAN_POINT('Ctrl Pts',(2.11583700529065,-0.827704675651187,0.493964776372216));
#7543=CARTESIAN_POINT('Ctrl Pts',(2.17948538095199,-0.862895030740277,-0.428930899822819));
#7544=CARTESIAN_POINT('Ctrl Pts',(2.24313375661331,-0.105624824409986,-0.958761037840773));
#7545=CARTESIAN_POINT('Ctrl Pts',(2.30678213227465,0.749868996341809,-0.605203607690351));
#7546=CARTESIAN_POINT('Ctrl Pts',(2.34921438271553,0.858976798481964,-0.0020476029672245));
#7547=CARTESIAN_POINT('Ctrl Pts',(2.37043050793598,0.773726326546544,0.255806069552507));
#7548=CARTESIAN_POINT('Ctrl Pts',(0.122919492064021,-0.391735495545771,
0.800079576859257));
#7549=CARTESIAN_POINT('Ctrl Pts',(0.144135617284465,-0.658371708018994,
0.669528976838104));
#7550=CARTESIAN_POINT('Ctrl Pts',(0.186567867725353,-1.04617702914432,0.123114203276511));
#7551=CARTESIAN_POINT('Ctrl Pts',(0.250216243386685,-0.668292674669318,
-0.81558853027891));
#7552=CARTESIAN_POINT('Ctrl Pts',(0.313864619048016,0.324656119420904,-1.00211549897901));
#7553=CARTESIAN_POINT('Ctrl Pts',(0.377512994709347,1.01878224613663,-0.268978036484718));
#7554=CARTESIAN_POINT('Ctrl Pts',(0.441161370370679,0.776847629751729,0.712044792777709));
#7555=CARTESIAN_POINT('Ctrl Pts',(0.50480974603201,-0.179162212450745,1.03831335101258));
#7556=CARTESIAN_POINT('Ctrl Pts',(0.568458121693342,-0.97045010230906,0.410523860222872));
#7557=CARTESIAN_POINT('Ctrl Pts',(0.632106497354674,-0.869894007381145,
-0.594651305427354));
#7558=CARTESIAN_POINT('Ctrl Pts',(0.695754873016005,0.0301439926800345,
-1.05326822380691));
#7559=CARTESIAN_POINT('Ctrl Pts',(0.759403248677337,0.902469041686343,-0.543921455352166));
#7560=CARTESIAN_POINT('Ctrl Pts',(0.823051624338668,0.945397711961052,0.465323137553205));
#7561=CARTESIAN_POINT('Ctrl Pts',(0.886699999999999,0.119469351883882,1.04691144995015));
#7562=CARTESIAN_POINT('Ctrl Pts',(0.950348375661332,-0.816254233537077,
0.666354631226919));
#7563=CARTESIAN_POINT('Ctrl Pts',(1.01399675132266,-1.00181165147662,-0.326608098769855));
#7564=CARTESIAN_POINT('Ctrl Pts',(1.077645126984,-0.266667861186703,-1.01940515872473));
#7565=CARTESIAN_POINT('Ctrl Pts',(1.14129350264533,0.713553044215432,-0.775332932522492));
#7566=CARTESIAN_POINT('Ctrl Pts',(1.20494187830666,1.03799324095032,0.18129838291439));
#7567=CARTESIAN_POINT('Ctrl Pts',(1.26859025396799,0.408480362652086,0.971309780599157));
#7568=CARTESIAN_POINT('Ctrl Pts',(1.33223862962932,-0.596440541908263,0.868652837371817));
#7569=CARTESIAN_POINT('Ctrl Pts',(1.39588700529065,-1.05321129994028,-0.0323274007792368));
#7570=CARTESIAN_POINT('Ctrl Pts',(1.45953538095198,-0.542042964705357,-0.903597283217423));
#7571=CARTESIAN_POINT('Ctrl Pts',(1.52318375661332,0.467282004678397,-0.944429437978354));
#7572=CARTESIAN_POINT('Ctrl Pts',(1.58683213227465,1.04715858930856,-0.1172960236414));
#7573=CARTESIAN_POINT('Ctrl Pts',(1.65048050793598,0.664657891865674,0.81763463530904));
#7574=CARTESIAN_POINT('Ctrl Pts',(1.71412888359731,-0.328685334495418,1.00113356102529));
#7575=CARTESIAN_POINT('Ctrl Pts',(1.77777725925864,-1.01995856504329,0.264547625938156));
#7576=CARTESIAN_POINT('Ctrl Pts',(1.84142563491997,-0.773846454525389,-0.715153323696768));
#7577=CARTESIAN_POINT('Ctrl Pts',(1.9050740105813,0.183445259101111,-1.03762883346474));
#7578=CARTESIAN_POINT('Ctrl Pts',(1.96872238624264,0.972168959713482,-0.406436655154973));
#7579=CARTESIAN_POINT('Ctrl Pts',(2.03237076190397,0.86738749634182,0.598191143741779));
#7580=CARTESIAN_POINT('Ctrl Pts',(2.0960191375653,-0.0344647747898869,1.05323891215213));
#7581=CARTESIAN_POINT('Ctrl Pts',(2.15966751322663,-0.904812658013209,0.539981946969935));
#7582=CARTESIAN_POINT('Ctrl Pts',(2.22331588888796,-0.94328130469512,-0.468889591891392));
#7583=CARTESIAN_POINT('Ctrl Pts',(2.28696426454929,-0.115464707326183,-1.04807807490724));
#7584=CARTESIAN_POINT('Ctrl Pts',(2.35061264021063,0.819725899467628,-0.661583655405445));
#7585=CARTESIAN_POINT('Ctrl Pts',(2.39304489065151,0.938998054583516,-0.00223835522237897));
#7586=CARTESIAN_POINT('Ctrl Pts',(2.41426101587196,0.845805750156719,0.279636658504581));
#7587=CARTESIAN_POINT('Ctrl Pts',(0.16675,-0.425119128515106,0.868262223680471));
#7588=CARTESIAN_POINT('Ctrl Pts',(0.187966125220444,-0.714478034118648,
0.726586123507844));
#7589=CARTESIAN_POINT('Ctrl Pts',(0.230398375661332,-1.13533205941097,0.13360597494956));
#7590=CARTESIAN_POINT('Ctrl Pts',(0.294046751322664,-0.725244463876405,
-0.885092847499123));
#7591=CARTESIAN_POINT('Ctrl Pts',(0.357695126983995,0.352323259251816,-1.08751561306413));
#7592=CARTESIAN_POINT('Ctrl Pts',(0.421343502645326,1.10560269760814,-0.291900299462976));
#7593=CARTESIAN_POINT('Ctrl Pts',(0.484991878306658,0.843050453952274,0.772725130122938));
#7594=CARTESIAN_POINT('Ctrl Pts',(0.54864025396799,-0.194430386028165,1.12679823995294));
#7595=CARTESIAN_POINT('Ctrl Pts',(0.612288629629321,-1.05315169662183,0.445508634466375));
#7596=CARTESIAN_POINT('Ctrl Pts',(0.675937005290653,-0.944026228215964,
-0.645327389547496));
#7597=CARTESIAN_POINT('Ctrl Pts',(0.739585380951984,0.0327128586605295,
-1.14302756448867));
#7598=CARTESIAN_POINT('Ctrl Pts',(0.803233756613316,0.979377301459615,-0.590274350190879));
#7599=CARTESIAN_POINT('Ctrl Pts',(0.866882132274647,1.02596434578673,0.504977896983606));
#7600=CARTESIAN_POINT('Ctrl Pts',(0.930530507935979,0.129650509934979,1.1361290674342));
#7601=CARTESIAN_POINT('Ctrl Pts',(0.994178883597311,-0.885815281876861,
0.723141260698177));
#7602=CARTESIAN_POINT('Ctrl Pts',(1.05782725925864,-1.08718587172874,-0.354441585952207));
#7603=CARTESIAN_POINT('Ctrl Pts',(1.12147563491997,-0.289393251415056,-1.10627869470211));
#7604=CARTESIAN_POINT('Ctrl Pts',(1.1851240105813,0.774361914494221,-0.841406674480209));
#7605=CARTESIAN_POINT('Ctrl Pts',(1.24877238624264,1.12645085016508,0.19674860057903));
#7606=CARTESIAN_POINT('Ctrl Pts',(1.31242076190397,0.443290990376694,1.05408463655106));
#7607=CARTESIAN_POINT('Ctrl Pts',(1.3760691375653,-0.647269104460033,0.942679285907431));
#7608=CARTESIAN_POINT('Ctrl Pts',(1.43971751322663,-1.14296578957972,-0.0350823364303007));
#7609=CARTESIAN_POINT('Ctrl Pts',(1.50336588888796,-0.588235774887451,-0.980601691543996));
#7610=CARTESIAN_POINT('Ctrl Pts',(1.5670142645493,0.507103698435367,-1.02491355565827));
#7611=CARTESIAN_POINT('Ctrl Pts',(1.63066264021062,1.13639726796712,-0.127291971025621));
#7612=CARTESIAN_POINT('Ctrl Pts',(1.69431101587196,0.721299925494264,0.887313321255395));
#7613=CARTESIAN_POINT('Ctrl Pts',(1.75795939153329,-0.356695843356533,1.08644999452333));
#7614=CARTESIAN_POINT('Ctrl Pts',(1.82160776719462,-1.10687926221396,0.287092330075636));
#7615=CARTESIAN_POINT('Ctrl Pts',(1.88525614285595,-0.839793519078488,-0.776098569523499));
#7616=CARTESIAN_POINT('Ctrl Pts',(1.94890451851729,0.199078433192889,-1.12605538793494));
#7617=CARTESIAN_POINT('Ctrl Pts',(2.01255289417861,1.05501703476484,-0.441073118470799));
#7618=CARTESIAN_POINT('Ctrl Pts',(2.07620126983995,0.941306112727917,0.649168892287031));
#7619=CARTESIAN_POINT('Ctrl Pts',(2.13984964550128,-0.0374018570942429,
1.14299575489962));
#7620=CARTESIAN_POINT('Ctrl Pts',(2.20349802116261,-0.981920640375234,0.585999117567654));
#7621=CARTESIAN_POINT('Ctrl Pts',(2.26714639682394,-1.02366757864996,-0.508848283959966));
#7622=CARTESIAN_POINT('Ctrl Pts',(2.33079477248527,-0.125304590242383,-1.1373951119737));
#7623=CARTESIAN_POINT('Ctrl Pts',(2.39444314814661,0.889582802593447,-0.717963703120541));
#7624=CARTESIAN_POINT('Ctrl Pts',(2.43687539858749,1.01901931068507,-0.00242910747753216));
#7625=CARTESIAN_POINT('Ctrl Pts',(2.45809152380794,0.917885173766894,0.303467247456655));
#7626=CARTESIAN_POINT('Ctrl Pts',(2.23776408311032,-0.965144827742031,-0.000120440973035392));
#7627=CARTESIAN_POINT('Ctrl Pts',(2.24755818768153,-0.965406583880997,-0.149376556276826));
#7628=CARTESIAN_POINT('Ctrl Pts',(2.25735229225274,-0.932889906533184,-0.298535024733765));
#7629=CARTESIAN_POINT('Ctrl Pts',(2.26714639682394,-0.866982590869575,-0.431131521707652));
#7630=CARTESIAN_POINT('Ctrl Pts',(2.28696426454929,-0.733622521609705,-0.699433725218841));
#7631=CARTESIAN_POINT('Ctrl Pts',(2.30678213227465,-0.463549677312364,-0.899925512525171));
#7632=CARTESIAN_POINT('Ctrl Pts',(2.3266,-0.168638277711113,-0.95359294643897));
#7633=CARTESIAN_POINT('',(0.16675,-0.429877377952346,-0.601104350279397));
#7634=CARTESIAN_POINT('Ctrl Pts',(0.16675,-0.430804868963501,-0.60198184778573));
#7635=CARTESIAN_POINT('Ctrl Pts',(0.16675,-0.445493125509025,-0.594569785083027));
#7636=CARTESIAN_POINT('Ctrl Pts',(0.16675,-0.459889646383086,-0.586644826880307));
#7637=CARTESIAN_POINT('Ctrl Pts',(0.16675,-0.473964720489372,-0.57821345471323));
#7638=CARTESIAN_POINT('Ctrl Pts',(0.16675,-0.502741553314337,-0.56097530836282));
#7639=CARTESIAN_POINT('Ctrl Pts',(0.16675,-0.530175722996942,-0.541623677822874));
#7640=CARTESIAN_POINT('Ctrl Pts',(0.16675,-0.556201153620589,-0.520414434550179));
#7641=CARTESIAN_POINT('Ctrl Pts',(0.16675,-0.569152311242204,-0.50985997892437));
#7642=CARTESIAN_POINT('Ctrl Pts',(0.16675,-0.581754443541687,-0.498844719299822));
#7643=CARTESIAN_POINT('Ctrl Pts',(0.16675,-0.593998024650347,-0.48739593053637));
#7644=CARTESIAN_POINT('Ctrl Pts',(0.16675,-0.600622288153534,-0.481201681248652));
#7645=CARTESIAN_POINT('Ctrl Pts',(0.16675,-0.607134985115756,-0.47488659859674));
#7646=CARTESIAN_POINT('Ctrl Pts',(0.16675,-0.61353303015818,-0.468457648512547));
#7647=CARTESIAN_POINT('Ctrl Pts',(0.16675,-0.638769508932995,-0.443099267746505));
#7648=CARTESIAN_POINT('Ctrl Pts',(0.16675,-0.662233574464342,-0.41596401595051));
#7649=CARTESIAN_POINT('Ctrl Pts',(0.16675,-0.683846027178802,-0.387333403011322));
#7650=CARTESIAN_POINT('Ctrl Pts',(0.16675,-0.692993268657504,-0.375215799623217));
#7651=CARTESIAN_POINT('Ctrl Pts',(0.16675,-0.701808594899562,-0.362829709101333));
#7652=CARTESIAN_POINT('Ctrl Pts',(0.16675,-0.710284757451846,-0.350193988883425));
#7653=CARTESIAN_POINT('Ctrl Pts',(0.16675,-0.715987571926311,-0.341692598341481));
#7654=CARTESIAN_POINT('Ctrl Pts',(0.16675,-0.721536841075486,-0.333078179490395));
#7655=CARTESIAN_POINT('Ctrl Pts',(0.16675,-0.7269301162124,-0.324356159333427));
#7656=CARTESIAN_POINT('Ctrl Pts',(0.16675,-0.731201614784776,-0.317448279482511));
#7657=CARTESIAN_POINT('Ctrl Pts',(0.16675,-0.735370253785842,-0.310480981392049));
#7658=CARTESIAN_POINT('Ctrl Pts',(0.16675,-0.739435066871342,-0.30345795973618));
#7659=CARTESIAN_POINT('Ctrl Pts',(0.16675,-0.758383963144114,-0.270718813783024));
#7660=CARTESIAN_POINT('Ctrl Pts',(0.16675,-0.775080533888005,-0.23676957537437));
#7661=CARTESIAN_POINT('Ctrl Pts',(0.16675,-0.789438812866396,-0.20191044083355));
#7662=CARTESIAN_POINT('Ctrl Pts',(0.16675,-0.803890891927935,-0.166823577765984));
#7663=CARTESIAN_POINT('Ctrl Pts',(0.16675,-0.815974925978725,-0.130813832498557));
#7664=CARTESIAN_POINT('Ctrl Pts',(0.16675,-0.825569104336731,-0.0941467411674717));
#7665=CARTESIAN_POINT('Ctrl Pts',(0.16675,-0.830507164894443,-0.0752744301980837));
#7666=CARTESIAN_POINT('Ctrl Pts',(0.16675,-0.834785003923765,-0.056227423211327));
#7667=CARTESIAN_POINT('Ctrl Pts',(0.16675,-0.838381312156127,-0.0370392251201134));
#7668=CARTESIAN_POINT('Ctrl Pts',(0.16675,-0.839815065498442,-0.0293893960819031));
#7669=CARTESIAN_POINT('Ctrl Pts',(0.16675,-0.841140278900315,-0.0217173226060706));
#7670=CARTESIAN_POINT('Ctrl Pts',(0.16675,-0.842353648640237,-0.0140391205839416));
#7671=CARTESIAN_POINT('Ctrl Pts',(0.16675,-0.84830136567568,0.0235980245219733));
#7672=CARTESIAN_POINT('Ctrl Pts',(0.16675,-0.851580929224255,0.0614634969090231));
#7673=CARTESIAN_POINT('Ctrl Pts',(0.16675,-0.85209621782855,0.0992883442314791));
#7674=CARTESIAN_POINT('Ctrl Pts',(0.16675,-0.852612773449657,0.137206197137624));
#7675=CARTESIAN_POINT('Ctrl Pts',(0.16675,-0.850352775477891,0.175084379198237));
#7676=CARTESIAN_POINT('Ctrl Pts',(0.16675,-0.845497452406605,0.212722826928005));
#7677=CARTESIAN_POINT('Ctrl Pts',(0.16675,-0.843191897632869,0.230595479595049));
#7678=CARTESIAN_POINT('Ctrl Pts',(0.16675,-0.840300368383401,0.248414272293587));
#7679=CARTESIAN_POINT('Ctrl Pts',(0.16675,-0.836838210915746,0.266158377798457));
#7680=CARTESIAN_POINT('Ctrl Pts',(0.16675,-0.834750433503057,0.276858567789101));
#7681=CARTESIAN_POINT('Ctrl Pts',(0.16675,-0.8324551019924,0.287531601952822));
#7682=CARTESIAN_POINT('Ctrl Pts',(0.16675,-0.829955143091132,0.298172905292354));
#7683=CARTESIAN_POINT('Ctrl Pts',(0.16675,-0.828112598179905,0.30601586595348));
#7684=CARTESIAN_POINT('Ctrl Pts',(0.16675,-0.8261610517908,0.313832300947477));
#7685=CARTESIAN_POINT('Ctrl Pts',(0.16675,-0.824102988029633,0.321618313365642));
#7686=CARTESIAN_POINT('Ctrl Pts',(0.16675,-0.813980647604896,0.359912884085456));
#7687=CARTESIAN_POINT('Ctrl Pts',(0.16675,-0.801282102136966,0.39748663728072));
#7688=CARTESIAN_POINT('Ctrl Pts',(0.16675,-0.786213950326801,0.434124784279322));
#7689=CARTESIAN_POINT('Ctrl Pts',(0.16675,-0.770797461365757,0.471609911577817));
#7690=CARTESIAN_POINT('Ctrl Pts',(0.16675,-0.752900368761167,0.508116767940505));
#7691=CARTESIAN_POINT('Ctrl Pts',(0.16675,-0.73268950485522,0.543417900500982));
#7692=CARTESIAN_POINT('Ctrl Pts',(0.16675,-0.722977720127076,0.560380906223174));
#7693=CARTESIAN_POINT('Ctrl Pts',(0.16675,-0.712730901400849,0.577065441373076));
#7694=CARTESIAN_POINT('Ctrl Pts',(0.16675,-0.70196345051309,0.593445288500454));
#7695=CARTESIAN_POINT('Ctrl Pts',(0.16675,-0.69721937633955,0.600662150739582));
#7696=CARTESIAN_POINT('Ctrl Pts',(0.16675,-0.692374202308048,0.60781985304043));
#7697=CARTESIAN_POINT('Ctrl Pts',(0.16675,-0.687429007292474,0.614916081051289));
#7698=CARTESIAN_POINT('Ctrl Pts',(0.16675,-0.682714384849053,0.621681443334934));
#7699=CARTESIAN_POINT('Ctrl Pts',(0.16675,-0.677914372753535,0.628382975887117));
#7700=CARTESIAN_POINT('Ctrl Pts',(0.16675,-0.673031649136193,0.635017507597753));
#7701=CARTESIAN_POINT('Ctrl Pts',(0.16675,-0.647947101036107,0.669101810306574));
#7702=CARTESIAN_POINT('Ctrl Pts',(0.16675,-0.620675093575939,0.701430768012057));
#7703=CARTESIAN_POINT('Ctrl Pts',(0.16675,-0.591410629122804,0.731767455494602));
#7704=CARTESIAN_POINT('Ctrl Pts',(0.16675,-0.562349677540372,0.761893173582266));
#7705=CARTESIAN_POINT('Ctrl Pts',(0.16675,-0.531323346456511,0.790055413649179));
#7706=CARTESIAN_POINT('Ctrl Pts',(0.16675,-0.498475258847458,0.81600537002847));
#7707=CARTESIAN_POINT('Ctrl Pts',(0.16675,-0.474945639402752,0.834593745871793));
#7708=CARTESIAN_POINT('Ctrl Pts',(0.16675,-0.450480256842734,0.85204668515908));
#7709=CARTESIAN_POINT('Ctrl Pts',(0.16675,-0.425119128515106,0.868262223680471));
#7710=CARTESIAN_POINT('Ctrl Pts',(0.166750000000001,-0.430804868963497,
-0.601981847785733));
#7711=CARTESIAN_POINT('Ctrl Pts',(0.186567867725353,-0.243806898334343,
-0.734404661945218));
#7712=CARTESIAN_POINT('Ctrl Pts',(0.227601860671149,0.281971713823132,-0.817954447443626));
#7713=CARTESIAN_POINT('Ctrl Pts',(0.289851978837389,0.845141343193606,-0.223133510528201));
#7714=CARTESIAN_POINT('Ctrl Pts',(0.35350035449872,0.644441981350638,0.590684118087253));
#7715=CARTESIAN_POINT('Ctrl Pts',(0.417148730160053,-0.148625865295904,
0.86134357313186));
#7716=CARTESIAN_POINT('Ctrl Pts',(0.468072798427941,-0.673818062791027,
0.444668243636764));
#7717=CARTESIAN_POINT('Ctrl Pts',(0.497780741475386,-0.738435342237461,
0.0992847338226311));
#7718=CARTESIAN_POINT('Ctrl Pts',(0.506272559302387,-0.737970603191613,
0.000391387174775012));
#7719=CARTESIAN_POINT('Origin',(0.16675,-2.39206768658147E-16,-5.43753587379397E-17));
#7720=CARTESIAN_POINT('',(0.16675,-0.96675,-1.1839272930757E-16));
#7721=CARTESIAN_POINT('Origin',(0.16675,0.,0.));
#7722=CARTESIAN_POINT('Origin',(0.16675,0.,0.));
#7723=CARTESIAN_POINT('',(0.16675,0.429877377952346,-0.601104350279397));
#7724=CARTESIAN_POINT('Ctrl Pts',(0.16675,0.426126619158378,0.869594511950287));
#7725=CARTESIAN_POINT('Ctrl Pts',(0.16675,0.444048204157592,0.858234946722552));
#7726=CARTESIAN_POINT('Ctrl Pts',(0.16675,0.461543004418397,0.846256521223882));
#7727=CARTESIAN_POINT('Ctrl Pts',(0.16675,0.478574283244814,0.833657137809103));
#7728=CARTESIAN_POINT('Ctrl Pts',(0.16675,0.509001100399174,0.811148015662355));
#7729=CARTESIAN_POINT('Ctrl Pts',(0.16675,0.537950187081889,0.786657827653572));
#7730=CARTESIAN_POINT('Ctrl Pts',(0.16675,0.565322184247078,0.760390349102262));
#7731=CARTESIAN_POINT('Ctrl Pts',(0.16675,0.580977577122889,0.745366684804185));
#7732=CARTESIAN_POINT('Ctrl Pts',(0.16675,0.596116548389853,0.729761264861267));
#7733=CARTESIAN_POINT('Ctrl Pts',(0.16675,0.610716049466699,0.713610321391338));
#7734=CARTESIAN_POINT('Ctrl Pts',(0.16675,0.618614322575215,0.704872724002614));
#7735=CARTESIAN_POINT('Ctrl Pts',(0.16675,0.626355539003896,0.695974058824874));
#7736=CARTESIAN_POINT('Ctrl Pts',(0.16675,0.633922359419622,0.686936797568183));
#7737=CARTESIAN_POINT('Ctrl Pts',(0.16675,0.660736193525347,0.654912299721848));
#7738=CARTESIAN_POINT('Ctrl Pts',(0.16675,0.685405961021896,0.62110392557575));
#7739=CARTESIAN_POINT('Ctrl Pts',(0.16675,0.707789016811858,0.585785643849129));
#7740=CARTESIAN_POINT('Ctrl Pts',(0.16675,0.720604135012202,0.565564635636181));
#7741=CARTESIAN_POINT('Ctrl Pts',(0.16675,0.73266879088414,0.544848299455873));
#7742=CARTESIAN_POINT('Ctrl Pts',(0.16675,0.743948601837455,0.523686665378094));
#7743=CARTESIAN_POINT('Ctrl Pts',(0.16675,0.748254387048905,0.51560874178174));
#7744=CARTESIAN_POINT('Ctrl Pts',(0.16675,0.752445749108298,0.507465930781441));
#7745=CARTESIAN_POINT('Ctrl Pts',(0.16675,0.756520547836615,0.499261024570285));
#7746=CARTESIAN_POINT('Ctrl Pts',(0.16675,0.760218791127057,0.491814340361506));
#7747=CARTESIAN_POINT('Ctrl Pts',(0.16675,0.76381903212279,0.484320354352865));
#7748=CARTESIAN_POINT('Ctrl Pts',(0.16675,0.767316849163895,0.476788329033034));
#7749=CARTESIAN_POINT('Ctrl Pts',(0.16675,0.784221971045724,0.440385680022968));
#7750=CARTESIAN_POINT('Ctrl Pts',(0.16675,0.798763409678176,0.403045533144019));
#7751=CARTESIAN_POINT('Ctrl Pts',(0.16675,0.810809555762439,0.365012096556293));
#7752=CARTESIAN_POINT('Ctrl Pts',(0.16675,0.822574175743337,0.327867525596231));
#7753=CARTESIAN_POINT('Ctrl Pts',(0.16675,0.831958863643941,0.290060609212317));
#7754=CARTESIAN_POINT('Ctrl Pts',(0.16675,0.838792795668049,0.251820776324567));
#7755=CARTESIAN_POINT('Ctrl Pts',(0.16675,0.841943056397508,0.23419323138815));
#7756=CARTESIAN_POINT('Ctrl Pts',(0.16675,0.844550600272548,0.216473818776536));
#7757=CARTESIAN_POINT('Ctrl Pts',(0.16675,0.846595044183084,0.198686089961416));
#7758=CARTESIAN_POINT('Ctrl Pts',(0.16675,0.847632483705251,0.189659824781285));
#7759=CARTESIAN_POINT('Ctrl Pts',(0.16675,0.848524888038838,0.180615982855043));
#7760=CARTESIAN_POINT('Ctrl Pts',(0.16675,0.849269357780081,0.171557746034708));
#7761=CARTESIAN_POINT('Ctrl Pts',(0.16675,0.849858399166255,0.164390663106622));
#7762=CARTESIAN_POINT('Ctrl Pts',(0.16675,0.850354504412772,0.157217608502542));
#7763=CARTESIAN_POINT('Ctrl Pts',(0.16675,0.85075616472443,0.150048288143431));
#7764=CARTESIAN_POINT('Ctrl Pts',(0.16675,0.852777542388293,0.113968288157456));
#7765=CARTESIAN_POINT('Ctrl Pts',(0.16675,0.852415681074446,0.0779207678734099));
#7766=CARTESIAN_POINT('Ctrl Pts',(0.16675,0.849542285446746,0.0420946893478588));
#7767=CARTESIAN_POINT('Ctrl Pts',(0.16675,0.846888448693774,0.00900611533130068));
#7768=CARTESIAN_POINT('Ctrl Pts',(0.16675,0.842091236173531,-0.0238940214503569));
#7769=CARTESIAN_POINT('Ctrl Pts',(0.16675,0.835242858213107,-0.0564423061914987));
#7770=CARTESIAN_POINT('Ctrl Pts',(0.16675,0.828597188620167,-0.0880271789097645));
#7771=CARTESIAN_POINT('Ctrl Pts',(0.16675,0.820019479587032,-0.119281105396314));
#7772=CARTESIAN_POINT('Ctrl Pts',(0.16675,0.809574742100293,-0.150037087823665));
#7773=CARTESIAN_POINT('Ctrl Pts',(0.16675,0.806977307323436,-0.157685595835918));
#7774=CARTESIAN_POINT('Ctrl Pts',(0.16675,0.804266871727105,-0.165295576565078));
#7775=CARTESIAN_POINT('Ctrl Pts',(0.16675,0.801446902967295,-0.172859717658773));
#7776=CARTESIAN_POINT('Ctrl Pts',(0.16675,0.788417061552043,-0.207810303033373));
#7777=CARTESIAN_POINT('Ctrl Pts',(0.16675,0.773040216963918,-0.241819733336439));
#7778=CARTESIAN_POINT('Ctrl Pts',(0.16675,0.755459606524671,-0.27465734479009));
#7779=CARTESIAN_POINT('Ctrl Pts',(0.16675,0.738098146793609,-0.307085619728946));
#7780=CARTESIAN_POINT('Ctrl Pts',(0.16675,0.718586548468597,-0.338371978906755));
#7781=CARTESIAN_POINT('Ctrl Pts',(0.16675,0.697030730379467,-0.368255555684412));
#7782=CARTESIAN_POINT('Ctrl Pts',(0.16675,0.686837234519666,-0.382387151845577));
#7783=CARTESIAN_POINT('Ctrl Pts',(0.16675,0.676186226245501,-0.396204408183039));
#7784=CARTESIAN_POINT('Ctrl Pts',(0.16675,0.665087296091944,-0.409675840453131));
#7785=CARTESIAN_POINT('Ctrl Pts',(0.16675,0.659050486142239,-0.417003076073115));
#7786=CARTESIAN_POINT('Ctrl Pts',(0.16675,0.652878889824389,-0.424230235737168));
#7787=CARTESIAN_POINT('Ctrl Pts',(0.16675,0.646590889416737,-0.431333603793795));
#7788=CARTESIAN_POINT('Ctrl Pts',(0.16675,0.623179046694935,-0.457781269976265));
#7789=CARTESIAN_POINT('Ctrl Pts',(0.16675,0.598112400326066,-0.482571263352541));
#7790=CARTESIAN_POINT('Ctrl Pts',(0.16675,0.571498848118781,-0.505481850389779));
#7791=CARTESIAN_POINT('Ctrl Pts',(0.16675,0.545853275924679,-0.527559140534908));
#7792=CARTESIAN_POINT('Ctrl Pts',(0.16675,0.518770427098911,-0.547891640792012));
#7793=CARTESIAN_POINT('Ctrl Pts',(0.16675,0.490330976191895,-0.566236195677696));
#7794=CARTESIAN_POINT('Ctrl Pts',(0.16675,0.470811033951257,-0.578827319640305));
#7795=CARTESIAN_POINT('Ctrl Pts',(0.16675,0.450651674365123,-0.590480997499789));
#7796=CARTESIAN_POINT('Ctrl Pts',(0.16675,0.429877377952347,-0.601104350279396));
#7797=CARTESIAN_POINT('Origin',(0.16675,0.,0.));
#7798=CARTESIAN_POINT('Origin',(-0.572772559302386,0.,0.));
#7799=CARTESIAN_POINT('Ctrl Pts',(0.16675,0.429877377952346,-0.601104350279397));
#7800=CARTESIAN_POINT('Ctrl Pts',(0.187966125220444,0.63020268545344,-0.45784250583252));
#7801=CARTESIAN_POINT('Ctrl Pts',(0.230398375661332,0.872834123616866,0.0422493396134374));
#7802=CARTESIAN_POINT('Ctrl Pts',(0.294046751322663,0.435343216015217,0.758672715515329));
#7803=CARTESIAN_POINT('Ctrl Pts',(0.357695126983995,-0.402604296286284,
0.775582665152948));
#7804=CARTESIAN_POINT('Ctrl Pts',(0.402088690108978,-0.728851347662273,
0.291015012319514));
#7805=CARTESIAN_POINT('Ctrl Pts',(0.425266128013518,-0.740099388012232,
0.0231307056922991));
#7806=CARTESIAN_POINT('Ctrl Pts',(0.427227440697614,-0.739952215624596,
0.000448480265853929));
#7807=CARTESIAN_POINT('Ctrl Pts',(0.0352584761920628,0.562359885162963,
-0.786356739692297));
#7808=CARTESIAN_POINT('Ctrl Pts',(0.0564746014125067,0.824422795889191,
-0.59894349460567));
#7809=CARTESIAN_POINT('Ctrl Pts',(0.0989068518533945,1.14183002571936,0.0552700258068862));
#7810=CARTESIAN_POINT('Ctrl Pts',(0.162555227514726,0.56951022203344,0.992485585554051));
#7811=CARTESIAN_POINT('Ctrl Pts',(0.226203603176058,-0.526681601400223,
1.01460695742438));
#7812=CARTESIAN_POINT('Ctrl Pts',(0.289851978837389,-1.13858611742084,0.105758482516412));
#7813=CARTESIAN_POINT('Ctrl Pts',(0.353500354498721,-0.704219736298823,
-0.901062052194361));
#7814=CARTESIAN_POINT('Ctrl Pts',(0.417148730160052,0.377418552482973,-1.07936663274048));
#7815=CARTESIAN_POINT('Ctrl Pts',(0.480797105821384,1.11215948537616,-0.265909044073595));
#7816=CARTESIAN_POINT('Ctrl Pts',(0.544445481482716,0.824805026575853,0.792041364549834));
#7817=CARTESIAN_POINT('Ctrl Pts',(0.608093857144046,-0.220584842909833,
1.12201795069882));
#7818=CARTESIAN_POINT('Ctrl Pts',(0.67174223280538,-1.06324405762272,0.420851095111989));
#7819=CARTESIAN_POINT('Ctrl Pts',(0.735390608466709,-0.928746646791689,
-0.667109467222269));
#7820=CARTESIAN_POINT('Ctrl Pts',(0.799038984128042,0.0593036878978548,
-1.14196384784033));
#7821=CARTESIAN_POINT('Ctrl Pts',(0.862687359789374,0.992851037269299,-0.567317079889055));
#7822=CARTESIAN_POINT('Ctrl Pts',(0.926335735450704,1.01393309871856,0.528716826373647));
#7823=CARTESIAN_POINT('Ctrl Pts',(0.989984111112038,0.103174080250363,1.13883974488377));
#7824=CARTESIAN_POINT('Ctrl Pts',(1.05363248677337,-0.902405499999265,0.702328792682534));
#7825=CARTESIAN_POINT('Ctrl Pts',(1.1172808624347,-1.07864214409527,-0.379647872875257));
#7826=CARTESIAN_POINT('Ctrl Pts',(1.18092923809603,-0.263567945093874,-1.1127143000303));
#7827=CARTESIAN_POINT('Ctrl Pts',(1.24457761375736,0.793734598360108,-0.823156588847623));
#7828=CARTESIAN_POINT('Ctrl Pts',(1.30822598941869,1.12156665624076,0.222911765209374));
#7829=CARTESIAN_POINT('Ctrl Pts',(1.37187436508003,0.418638643118788,1.06411584982561));
#7830=CARTESIAN_POINT('Ctrl Pts',(1.43552274074136,-0.669033089544462,0.927359982025442));
#7831=CARTESIAN_POINT('Ctrl Pts',(1.49917111640269,-1.14183980758859,-0.0616741854150761));
#7832=CARTESIAN_POINT('Ctrl Pts',(1.56281949206402,-0.565254094904384,-0.994025233767431));
#7833=CARTESIAN_POINT('Ctrl Pts',(1.62646786772535,0.530819035010965,-1.01283588367238));
#7834=CARTESIAN_POINT('Ctrl Pts',(1.69011624338668,1.1390530241903,-0.100805646716435));
#7835=CARTESIAN_POINT('Ctrl Pts',(1.75376461904802,0.700451549597658,0.903852632500549));
#7836=CARTESIAN_POINT('Ctrl Pts',(1.81741299470935,-0.381880694848822,1.07786826185974));
#7837=CARTESIAN_POINT('Ctrl Pts',(1.88106137037068,-1.1132685844485,0.261226720517503));
#7838=CARTESIAN_POINT('Ctrl Pts',(1.94470974603201,-0.821489124128327,-0.795382116074246));
#7839=CARTESIAN_POINT('Ctrl Pts',(2.00835812169334,0.225204422399939,-1.12121417536036));
#7840=CARTESIAN_POINT('Ctrl Pts',(2.07200649735467,1.06504845822836,-0.416215070646207));
#7841=CARTESIAN_POINT('Ctrl Pts',(2.13565487301601,0.925843278457432,0.670548291357633));
#7842=CARTESIAN_POINT('Ctrl Pts',(2.19930324867734,-0.0637982312897449,
1.14249696551783));
#7843=CARTESIAN_POINT('Ctrl Pts',(2.26295162433867,-0.995715013444193,0.561588991513182));
#7844=CARTESIAN_POINT('Ctrl Pts',(2.30538387477956,-1.00549420213374,-0.165492191923457));
#7845=CARTESIAN_POINT('Ctrl Pts',(2.3266,-0.855344277194458,-0.450546035351206));
#7846=CARTESIAN_POINT('Ctrl Pts',(0.0790889841280419,0.51819904942609,-0.724605943221331));
#7847=CARTESIAN_POINT('Ctrl Pts',(0.100305109348486,0.759682759077274,-0.551909831681287));
#7848=CARTESIAN_POINT('Ctrl Pts',(0.142737359789374,1.05216472501853,0.050929797075736));
#7849=CARTESIAN_POINT('Ctrl Pts',(0.206385735450705,0.524787886694032,0.914547962207811));
#7850=CARTESIAN_POINT('Ctrl Pts',(0.270034111112037,-0.485322499695577,
0.934932193333899));
#7851=CARTESIAN_POINT('Ctrl Pts',(0.333682486773368,-1.04917555342029,0.0974535107404919));
#7852=CARTESIAN_POINT('Ctrl Pts',(0.3973308624347,-0.648918970867547,-0.830303709848955));
#7853=CARTESIAN_POINT('Ctrl Pts',(0.460979238096032,0.347780736664339,-0.994606439444508));
#7854=CARTESIAN_POINT('Ctrl Pts',(0.524627613757363,1.02482414435576,-0.245027814942394));
#7855=CARTESIAN_POINT('Ctrl Pts',(0.588275989418695,0.760034974062225,0.729844167488813));
#7856=CARTESIAN_POINT('Ctrl Pts',(0.651924365080026,-0.203262819645385,
1.03390844694167));
#7857=CARTESIAN_POINT('Ctrl Pts',(0.715572740741358,-0.979749933280485,
0.387802621045355));
#7858=CARTESIAN_POINT('Ctrl Pts',(0.77922111640269,-0.855814296543672,-0.614722886355148));
#7859=CARTESIAN_POINT('Ctrl Pts',(0.842869492064021,0.054646704907169,-1.05228803839437));
#7860=CARTESIAN_POINT('Ctrl Pts',(0.906517867725352,0.914884715835602,-0.522766966986812));
#7861=CARTESIAN_POINT('Ctrl Pts',(0.970166243386684,0.934311251211222,0.487197903106137));
#7862=CARTESIAN_POINT('Ctrl Pts',(1.03381461904802,0.0950720556741984,1.04940926409856));
#7863=CARTESIAN_POINT('Ctrl Pts',(1.09746299470935,-0.831541659770034,0.647176518729099));
#7864=CARTESIAN_POINT('Ctrl Pts',(1.16111137037068,-0.993938843235788,-0.349834993624386));
#7865=CARTESIAN_POINT('Ctrl Pts',(1.22475974603201,-0.242870557111759,-1.0253353906839));
#7866=CARTESIAN_POINT('Ctrl Pts',(1.28840812169334,0.731404435520177,-0.758515984379027));
#7867=CARTESIAN_POINT('Ctrl Pts',(1.35205649735468,1.03349259160535,0.205407014058117));
#7868=CARTESIAN_POINT('Ctrl Pts',(1.415704873016,0.385763907847585,0.980553265635359));
#7869=CARTESIAN_POINT('Ctrl Pts',(1.47935324867734,-0.616495451015456,0.854536523390396));
#7870=CARTESIAN_POINT('Ctrl Pts',(1.54300162433866,-1.05217373873994,-0.0568310526753888));
#7871=CARTESIAN_POINT('Ctrl Pts',(1.60665,-0.520865983495204,-0.915966705367969));
#7872=CARTESIAN_POINT('Ctrl Pts',(1.67029837566133,0.489135030106648,-0.933300197953434));
#7873=CARTESIAN_POINT('Ctrl Pts',(1.73394675132267,1.0496057950689,-0.0928896098093842));
#7874=CARTESIAN_POINT('Ctrl Pts',(1.79759512698399,0.645446691250665,0.832875152265396));
#7875=CARTESIAN_POINT('Ctrl Pts',(1.86124350264533,-0.351892477194545,0.993225732202447));
#7876=CARTESIAN_POINT('Ctrl Pts',(1.92489187830666,-1.02584614841431,0.240713183547288));
#7877=CARTESIAN_POINT('Ctrl Pts',(1.98854025396799,-0.756979461850859,-0.732922577435883));
#7878=CARTESIAN_POINT('Ctrl Pts',(2.05218862962932,0.20751963412252,-1.03316779024241));
#7879=CARTESIAN_POINT('Ctrl Pts',(2.11583700529065,0.981412638432993,-0.383530652978877));
#7880=CARTESIAN_POINT('Ctrl Pts',(2.17948538095198,0.853138923085075,0.617891667495313));
#7881=CARTESIAN_POINT('Ctrl Pts',(2.24313375661332,-0.0587883020849396,
1.05277929155983));
#7882=CARTESIAN_POINT('Ctrl Pts',(2.30678213227465,-0.917523790511027,0.517488692291692));
#7883=CARTESIAN_POINT('Ctrl Pts',(2.34921438271553,-0.926535041876538,-0.152496468551139));
#7884=CARTESIAN_POINT('Ctrl Pts',(2.37043050793598,-0.788176047169102,-0.415165685536108));
#7885=CARTESIAN_POINT('Ctrl Pts',(0.122919492064021,0.474038213689218,-0.662855146750364));
#7886=CARTESIAN_POINT('Ctrl Pts',(0.144135617284465,0.694942722265357,-0.504876168756904));
#7887=CARTESIAN_POINT('Ctrl Pts',(0.186567867725353,0.962499424317696,0.0465895683445864));
#7888=CARTESIAN_POINT('Ctrl Pts',(0.250216243386684,0.480065551354624,0.83661033886157));
#7889=CARTESIAN_POINT('Ctrl Pts',(0.313864619048015,-0.443963397990931,
0.855257429243423));
#7890=CARTESIAN_POINT('Ctrl Pts',(0.377512994709348,-0.959764989419737,
0.089148538964571));
#7891=CARTESIAN_POINT('Ctrl Pts',(0.441161370370679,-0.593618205436271,
-0.759545367503548));
#7892=CARTESIAN_POINT('Ctrl Pts',(0.504809746032011,0.318142920845704,-0.909846246148534));
#7893=CARTESIAN_POINT('Ctrl Pts',(0.568458121693342,0.937488803335355,-0.224146585811195));
#7894=CARTESIAN_POINT('Ctrl Pts',(0.632106497354674,0.695264921548596,0.667646970427793));
#7895=CARTESIAN_POINT('Ctrl Pts',(0.695754873016005,-0.185940796380938,
0.945798943184532));
#7896=CARTESIAN_POINT('Ctrl Pts',(0.759403248677337,-0.896255808938247,
0.35475414697872));
#7897=CARTESIAN_POINT('Ctrl Pts',(0.823051624338669,-0.782881946295657,
-0.562336305488026));
#7898=CARTESIAN_POINT('Ctrl Pts',(0.8867,0.049989721916484,-0.962612228948414));
#7899=CARTESIAN_POINT('Ctrl Pts',(0.950348375661331,0.836918394401904,-0.478216854084567));
#7900=CARTESIAN_POINT('Ctrl Pts',(1.01399675132266,0.854689403703885,0.445678979838627));
#7901=CARTESIAN_POINT('Ctrl Pts',(1.077645126984,0.0869700310980342,0.959978783313364));
#7902=CARTESIAN_POINT('Ctrl Pts',(1.14129350264533,-0.760677819540801,0.592024244775666));
#7903=CARTESIAN_POINT('Ctrl Pts',(1.20494187830666,-0.909235542376312,-0.320022114373516));
#7904=CARTESIAN_POINT('Ctrl Pts',(1.26859025396799,-0.222173169129643,-0.937956481337493));
#7905=CARTESIAN_POINT('Ctrl Pts',(1.33223862962932,0.669074272680244,-0.693875379910431));
#7906=CARTESIAN_POINT('Ctrl Pts',(1.39588700529065,0.945418526969947,0.18790226290686));
#7907=CARTESIAN_POINT('Ctrl Pts',(1.45953538095198,0.352889172576383,0.896990681445106));
#7908=CARTESIAN_POINT('Ctrl Pts',(1.52318375661332,-0.56395781248645,0.781713064755349));
#7909=CARTESIAN_POINT('Ctrl Pts',(1.58683213227465,-0.962507669891289,-0.0519879199356997));
#7910=CARTESIAN_POINT('Ctrl Pts',(1.65048050793598,-0.476477872086025,-0.837908176968511));
#7911=CARTESIAN_POINT('Ctrl Pts',(1.71412888359731,0.447451025202331,-0.853764512234482));
#7912=CARTESIAN_POINT('Ctrl Pts',(1.77777725925864,0.960158565947502,-0.0849735729023353));
#7913=CARTESIAN_POINT('Ctrl Pts',(1.84142563491997,0.590441832903672,0.761897672030244));
#7914=CARTESIAN_POINT('Ctrl Pts',(1.9050740105813,-0.321904259540268,0.908583202545158));
#7915=CARTESIAN_POINT('Ctrl Pts',(1.96872238624264,-0.938423712380128,0.220199646577074));
#7916=CARTESIAN_POINT('Ctrl Pts',(2.03237076190397,-0.692469799573391,-0.670463038797522));
#7917=CARTESIAN_POINT('Ctrl Pts',(2.0960191375653,0.189834845845101,-0.945121405124467));
#7918=CARTESIAN_POINT('Ctrl Pts',(2.15966751322663,0.897776818637627,-0.350846235311547));
#7919=CARTESIAN_POINT('Ctrl Pts',(2.22331588888796,0.780434567712718,0.565235043632989));
#7920=CARTESIAN_POINT('Ctrl Pts',(2.2869642645493,-0.0537783728801341,0.963061617601832));
#7921=CARTESIAN_POINT('Ctrl Pts',(2.35061264021062,-0.839332567577861,0.4733883930702));
#7922=CARTESIAN_POINT('Ctrl Pts',(2.39304489065151,-0.847575881619333,-0.13950074517882));
#7923=CARTESIAN_POINT('Ctrl Pts',(2.41426101587196,-0.721007817143747,-0.379785335721011));
#7924=CARTESIAN_POINT('Ctrl Pts',(0.16675,0.429877377952346,-0.601104350279397));
#7925=CARTESIAN_POINT('Ctrl Pts',(0.187966125220444,0.63020268545344,-0.45784250583252));
#7926=CARTESIAN_POINT('Ctrl Pts',(0.230398375661332,0.872834123616866,0.0422493396134374));
#7927=CARTESIAN_POINT('Ctrl Pts',(0.294046751322663,0.435343216015217,0.758672715515329));
#7928=CARTESIAN_POINT('Ctrl Pts',(0.357695126983995,-0.402604296286284,
0.775582665152948));
#7929=CARTESIAN_POINT('Ctrl Pts',(0.421343502645327,-0.870354425419187,
0.0808435671886495));
#7930=CARTESIAN_POINT('Ctrl Pts',(0.484991878306658,-0.538317440004995,
-0.688787025158141));
#7931=CARTESIAN_POINT('Ctrl Pts',(0.54864025396799,0.288505105027068,-0.825086052852563));
#7932=CARTESIAN_POINT('Ctrl Pts',(0.612288629629321,0.850153462314954,-0.203265356679994));
#7933=CARTESIAN_POINT('Ctrl Pts',(0.675937005290653,0.630494869034967,0.605449773366773));
#7934=CARTESIAN_POINT('Ctrl Pts',(0.739585380951984,-0.168618773116491,
0.857689439427387));
#7935=CARTESIAN_POINT('Ctrl Pts',(0.803233756613316,-0.81276168459601,0.321705672912086));
#7936=CARTESIAN_POINT('Ctrl Pts',(0.866882132274647,-0.70994959604764,-0.509949724620904));
#7937=CARTESIAN_POINT('Ctrl Pts',(0.93053050793598,0.0453327389257982,-0.872936419502457));
#7938=CARTESIAN_POINT('Ctrl Pts',(0.99417888359731,0.758952072968206,-0.433666741182324));
#7939=CARTESIAN_POINT('Ctrl Pts',(1.05782725925864,0.775067556196549,0.404160056571117));
#7940=CARTESIAN_POINT('Ctrl Pts',(1.12147563491997,0.0788680065218695,0.870548302528163));
#7941=CARTESIAN_POINT('Ctrl Pts',(1.1851240105813,-0.689813979311569,0.536871970822231));
#7942=CARTESIAN_POINT('Ctrl Pts',(1.24877238624264,-0.824532241516836,-0.290209235122645));
#7943=CARTESIAN_POINT('Ctrl Pts',(1.31242076190396,-0.201475781147527,-0.850577571991093));
#7944=CARTESIAN_POINT('Ctrl Pts',(1.37606913756531,0.606744109840312,-0.629234775441834));
#7945=CARTESIAN_POINT('Ctrl Pts',(1.43971751322663,0.857344462334542,0.170397511755603));
#7946=CARTESIAN_POINT('Ctrl Pts',(1.50336588888797,0.32001443730518,0.813428097254852));
#7947=CARTESIAN_POINT('Ctrl Pts',(1.56701426454929,-0.511420173957444,0.708889606120302));
#7948=CARTESIAN_POINT('Ctrl Pts',(1.63066264021063,-0.872841601042637,-0.0471447871960115));
#7949=CARTESIAN_POINT('Ctrl Pts',(1.69431101587196,-0.432089760676844,-0.759849648569051));
#7950=CARTESIAN_POINT('Ctrl Pts',(1.75795939153329,0.405767020298013,-0.774228826515532));
#7951=CARTESIAN_POINT('Ctrl Pts',(1.82160776719462,0.870711336826102,-0.0770575359952864));
#7952=CARTESIAN_POINT('Ctrl Pts',(1.88525614285595,0.535436974556678,0.690920191795093));
#7953=CARTESIAN_POINT('Ctrl Pts',(1.94890451851728,-0.291916041885991,0.823940672887867));
#7954=CARTESIAN_POINT('Ctrl Pts',(2.01255289417862,-0.851001276345943,0.199686109606861));
#7955=CARTESIAN_POINT('Ctrl Pts',(2.07620126983995,-0.627960137295923,-0.60800350015916));
#7956=CARTESIAN_POINT('Ctrl Pts',(2.13984964550128,0.172150057567682,-0.857075020006521));
#7957=CARTESIAN_POINT('Ctrl Pts',(2.20349802116261,0.814140998842262,-0.318161817644216));
#7958=CARTESIAN_POINT('Ctrl Pts',(2.26714639682394,0.707730212340359,0.512578419770666));
#7959=CARTESIAN_POINT('Ctrl Pts',(2.33079477248527,-0.0487684436753277,
0.873343943643834));
#7960=CARTESIAN_POINT('Ctrl Pts',(2.39444314814661,-0.761141344644696,0.429288093848709));
#7961=CARTESIAN_POINT('Ctrl Pts',(2.43687539858749,-0.768616721362127,-0.126505021806502));
#7962=CARTESIAN_POINT('Ctrl Pts',(2.45809152380794,-0.653839587118391,-0.344404985905914));
#7963=CARTESIAN_POINT('Ctrl Pts',(2.3266,-0.855344277194458,-0.450546035351206));
#7964=CARTESIAN_POINT('Ctrl Pts',(2.31631197229656,-0.928154301239586,-0.312319011910983));
#7965=CARTESIAN_POINT('Ctrl Pts',(2.30602394459312,-0.964507862952725,-0.155636376663986));
#7966=CARTESIAN_POINT('Ctrl Pts',(2.29573591688968,-0.964651808581398,0.000865815094782327));
#7967=CARTESIAN_POINT('Origin',(0.,-9.54517714852416E-17,-0.519615242270663));
#7968=CARTESIAN_POINT('',(0.,-9.54517714852416E-17,-0.519615242270663));
#7969=CARTESIAN_POINT('',(0.,0.45,-0.259807621135332));
#7970=CARTESIAN_POINT('',(0.,0.4125,-0.281458256229943));
#7971=CARTESIAN_POINT('',(1.2,-6.93889390390723E-17,-0.519615242270663));
#7972=CARTESIAN_POINT('',(0.,-9.54517714852416E-17,-0.519615242270663));
#7973=CARTESIAN_POINT('',(1.2,0.45,-0.259807621135332));
#7974=CARTESIAN_POINT('',(1.2,-9.54517714852416E-17,-0.519615242270663));
#7975=CARTESIAN_POINT('',(0.,0.45,-0.259807621135332));
#7976=CARTESIAN_POINT('Origin',(0.,-0.45,-0.259807621135332));
#7977=CARTESIAN_POINT('',(0.,-0.45,-0.259807621135332));
#7978=CARTESIAN_POINT('',(0.,-0.0375000000000001,-0.497964607176052));
#7979=CARTESIAN_POINT('',(1.2,-0.45,-0.259807621135332));
#7980=CARTESIAN_POINT('',(0.,-0.45,-0.259807621135332));
#7981=CARTESIAN_POINT('',(1.2,-0.45,-0.259807621135332));
#7982=CARTESIAN_POINT('Origin',(0.,-0.45,0.259807621135332));
#7983=CARTESIAN_POINT('',(0.,-0.45,0.259807621135332));
#7984=CARTESIAN_POINT('',(0.,-0.45,0.129903810567666));
#7985=CARTESIAN_POINT('',(1.2,-0.45,0.259807621135332));
#7986=CARTESIAN_POINT('',(0.,-0.45,0.259807621135332));
#7987=CARTESIAN_POINT('',(1.2,-0.45,0.259807621135332));
#7988=CARTESIAN_POINT('Origin',(0.,3.18172571617472E-17,0.519615242270663));
#7989=CARTESIAN_POINT('',(0.,3.18172571617472E-17,0.519615242270663));
#7990=CARTESIAN_POINT('',(0.,0.1875,0.627868417743718));
#7991=CARTESIAN_POINT('',(1.2,0.,0.519615242270663));
#7992=CARTESIAN_POINT('',(0.,3.18172571617472E-17,0.519615242270663));
#7993=CARTESIAN_POINT('',(1.2,3.18172571617472E-17,0.519615242270663));
#7994=CARTESIAN_POINT('Origin',(0.,0.45,0.259807621135332));
#7995=CARTESIAN_POINT('',(0.,0.45,0.259807621135332));
#7996=CARTESIAN_POINT('',(0.,0.6375,0.151554445662277));
#7997=CARTESIAN_POINT('',(1.2,0.45,0.259807621135332));
#7998=CARTESIAN_POINT('',(0.,0.45,0.259807621135332));
#7999=CARTESIAN_POINT('',(1.2,0.45,0.259807621135332));
#8000=CARTESIAN_POINT('Origin',(0.,0.45,-0.259807621135332));
#8001=CARTESIAN_POINT('',(0.,0.45,-0.129903810567666));
#8002=CARTESIAN_POINT('',(1.2,0.45,-0.259807621135332));
#8003=CARTESIAN_POINT('Origin',(1.2,0.,-6.93889390390723E-17));
#8004=CARTESIAN_POINT('Origin',(0.,0.8,0.));
#8005=CARTESIAN_POINT('',(6.93889390390723E-17,-0.8,-9.79717439317883E-17));
#8006=CARTESIAN_POINT('Origin',(0.,0.,0.));
#8007=CARTESIAN_POINT('Origin',(0.1,0.,0.));
#8008=CARTESIAN_POINT('',(0.1,-0.9,-1.10218211923262E-16));
#8009=CARTESIAN_POINT('Origin',(1.25,0.,0.));
#8010=CARTESIAN_POINT('Origin',(2.3266,0.,0.));
#8011=CARTESIAN_POINT('Origin',(2.4,0.,0.));
#8012=CARTESIAN_POINT('',(2.5,-0.75,-9.18485099360515E-17));
#8013=CARTESIAN_POINT('Origin',(2.5,0.,0.));
#8014=CARTESIAN_POINT('',(2.4,-0.875,-1.07156594925393E-16));
#8015=CARTESIAN_POINT('Origin',(2.5,0.,0.));
#8016=CARTESIAN_POINT('',(0.,0.,0.));
#8017=CARTESIAN_POINT('Origin',(-1.1,0.,0.));
#8018=CARTESIAN_POINT('',(-2.09010734985006,-1.21555704018822,0.00101556544434535));
#8019=CARTESIAN_POINT('',(-2.15489265014994,-1.21581627598942,0.00130132384810224));
#8020=CARTESIAN_POINT('',(-1.1,-1.215,-1.48794586096403E-16));
#8021=CARTESIAN_POINT('',(-2.235,0.531593232241059,1.09337941589937));
#8022=CARTESIAN_POINT('Ctrl Pts',(-2.09010734985006,-1.21555704018822,0.00101556544434535));
#8023=CARTESIAN_POINT('Ctrl Pts',(-2.09435627684546,-1.21616855233654,0.0729895168668011));
#8024=CARTESIAN_POINT('Ctrl Pts',(-2.09860520384087,-1.2103032966511,0.144859657339869));
#8025=CARTESIAN_POINT('Ctrl Pts',(-2.10285413083627,-1.19759745787725,0.215493040591908));
#8026=CARTESIAN_POINT('Ctrl Pts',(-2.12621917673445,-1.1277274633005,0.603909279188963));
#8027=CARTESIAN_POINT('Ctrl Pts',(-2.14958422263263,-0.85100159321999,0.954926586373963));
#8028=CARTESIAN_POINT('Ctrl Pts',(-2.17294926853081,-0.489637107432698,
1.11385746442067));
#8029=CARTESIAN_POINT('Ctrl Pts',(-2.19363284568721,-0.169744295925529,
1.25454878139639));
#8030=CARTESIAN_POINT('Ctrl Pts',(-2.2143164228436,0.216474938558358,1.24471299392075));
#8031=CARTESIAN_POINT('Ctrl Pts',(-2.235,0.532202955181985,1.09392695412892));
#8032=CARTESIAN_POINT('',(-2.235,-0.530983509300121,1.09283187766981));
#8033=CARTESIAN_POINT('Origin',(-2.235,0.,0.));
#8034=CARTESIAN_POINT('Ctrl Pts',(-2.235,-0.53098350930012,1.09283187766981));
#8035=CARTESIAN_POINT('Ctrl Pts',(-2.21163495410182,-0.887506341491207,
0.919605100110861));
#8036=CARTESIAN_POINT('Ctrl Pts',(-2.18826990820364,-1.15001549756272,0.560130039467285));
#8037=CARTESIAN_POINT('Ctrl Pts',(-2.16490486230546,-1.20483997833738,0.169869648085053));
#8038=CARTESIAN_POINT('Ctrl Pts',(-2.16156745825362,-1.21267096848714,0.114125840983309));
#8039=CARTESIAN_POINT('Ctrl Pts',(-2.15823005420178,-1.21626466312913,0.0577539348489441));
#8040=CARTESIAN_POINT('Ctrl Pts',(-2.15489265014994,-1.21581627598942,0.00130132384810224));
#8041=CARTESIAN_POINT('Origin',(-1.1,0.,0.));
#8042=CARTESIAN_POINT('',(-1.64010734985006,-1.21347552231432,-0.000575546447129233));
#8043=CARTESIAN_POINT('',(-1.70489265014994,-1.21328542726779,-0.000363737954992407));
#8044=CARTESIAN_POINT('',(-1.1,-1.215,-1.48794586096403E-16));
#8045=CARTESIAN_POINT('Ctrl Pts',(-1.64010734985006,-1.21347552231432,-0.000575546447129233));
#8046=CARTESIAN_POINT('Ctrl Pts',(-1.65416600145638,-1.21240787552406,0.238620955458428));
#8047=CARTESIAN_POINT('Ctrl Pts',(-1.6682246530627,-1.14377867336048,0.478382638558954));
#8048=CARTESIAN_POINT('Ctrl Pts',(-1.68228330466901,-1.01186572903878,0.675872676498389));
#8049=CARTESIAN_POINT('Ctrl Pts',(-1.7056483505672,-0.792630479105178,1.00409503594676));
#8050=CARTESIAN_POINT('Ctrl Pts',(-1.72901339646538,-0.398596571949964,
1.21555712552604));
#8051=CARTESIAN_POINT('Ctrl Pts',(-1.75237844236356,-0.00388959740550279,
1.21682095992699));
#8052=CARTESIAN_POINT('Ctrl Pts',(-1.77574348826174,0.39081737713896,1.21808479432795));
#8053=CARTESIAN_POINT('Ctrl Pts',(-1.79910853415992,0.78619741907267,1.00915037355058));
#8054=CARTESIAN_POINT('Ctrl Pts',(-1.8224735800581,1.00752575948006,0.682330574304518));
#8055=CARTESIAN_POINT('Ctrl Pts',(-1.84583862595628,1.22885409988745,0.355510775058457));
#8056=CARTESIAN_POINT('Ctrl Pts',(-1.86920367185446,1.27613073876853,-0.0891944026562985));
#8057=CARTESIAN_POINT('Ctrl Pts',(-1.89256871775264,1.12846908484488,-0.455233278205789));
#8058=CARTESIAN_POINT('Ctrl Pts',(-1.91593376365082,0.980807430921236,-0.821272153755278));
#8059=CARTESIAN_POINT('Ctrl Pts',(-1.939298809549,0.638207484192875,-1.1086447271395));
#8060=CARTESIAN_POINT('Ctrl Pts',(-1.96266385544718,0.252056972817938,-1.19042038674822));
#8061=CARTESIAN_POINT('Ctrl Pts',(-1.98602890134536,-0.134093538557,-1.27219604635694));
#8062=CARTESIAN_POINT('Ctrl Pts',(-2.00939394724354,-0.563794614578515,
-1.14837479219015));
#8063=CARTESIAN_POINT('Ctrl Pts',(-2.03275899314173,-0.847138093052768,
-0.873556580102204));
#8064=CARTESIAN_POINT('Ctrl Pts',(-2.0518751120445,-1.07895564001776,-0.648713982239761));
#8065=CARTESIAN_POINT('Ctrl Pts',(-2.07099123094728,-1.21280581877384,-0.322798568049416));
#8066=CARTESIAN_POINT('Ctrl Pts',(-2.09010734985006,-1.21555704018822,0.00101556544434535));
#8067=CARTESIAN_POINT('Ctrl Pts',(-2.15489265014994,-1.21581627598942,0.00130132384810224));
#8068=CARTESIAN_POINT('Ctrl Pts',(-2.1348650083036,-1.21312552086863,-0.337468767172928));
#8069=CARTESIAN_POINT('Ctrl Pts',(-2.11483736645726,-1.06487305501001,-0.679145167136663));
#8070=CARTESIAN_POINT('Ctrl Pts',(-2.09480972461092,-0.81324537235474,-0.90543373177546));
#8071=CARTESIAN_POINT('Ctrl Pts',(-2.07144467871274,-0.519686480119644,
-1.16943099813285));
#8072=CARTESIAN_POINT('Ctrl Pts',(-2.04807963281455,-0.0854288901716521,
-1.27637980872674));
#8073=CARTESIAN_POINT('Ctrl Pts',(-2.02471458691637,0.297352750944294,-1.17983198073104));
#8074=CARTESIAN_POINT('Ctrl Pts',(-2.00134954101819,0.68013439206024,-1.08328415273534));
#8075=CARTESIAN_POINT('Ctrl Pts',(-1.97798449512001,1.01144008434414,-0.783239686150053));
#8076=CARTESIAN_POINT('Ctrl Pts',(-1.95461944922183,1.14500372357387,-0.411877774273037));
#8077=CARTESIAN_POINT('Ctrl Pts',(-1.93125440332365,1.27856736280359,-0.0405158623960201));
#8078=CARTESIAN_POINT('Ctrl Pts',(-1.90788935742547,1.21438894897914,0.402163494772724));
#8079=CARTESIAN_POINT('Ctrl Pts',(-1.88452431152729,0.98075572302807,0.720320851177092));
#8080=CARTESIAN_POINT('Ctrl Pts',(-1.86115926562911,0.747122497076996,1.03847820758146));
#8081=CARTESIAN_POINT('Ctrl Pts',(-1.83779421973093,0.344034458999299,1.23211356322145));
#8082=CARTESIAN_POINT('Ctrl Pts',(-1.81442917383275,-0.050341458175738,
1.21577086315243));
#8083=CARTESIAN_POINT('Ctrl Pts',(-1.79106412793457,-0.444717375350775,
1.19942816308341));
#8084=CARTESIAN_POINT('Ctrl Pts',(-1.76769908203638,-0.83038117162315,0.973107407305383));
#8085=CARTESIAN_POINT('Ctrl Pts',(-1.7443340361382,-1.03692497416749,0.63676228257843));
#8086=CARTESIAN_POINT('Ctrl Pts',(-1.73118690747545,-1.15314378916056,0.447506389431653));
#8087=CARTESIAN_POINT('Ctrl Pts',(-1.71803977881269,-1.21265091085685,0.223415366285508));
#8088=CARTESIAN_POINT('Ctrl Pts',(-1.70489265014994,-1.21328542726779,-0.000363737954992407));
#8089=CARTESIAN_POINT('Origin',(-1.1,0.,0.));
#8090=CARTESIAN_POINT('',(-1.19010734985006,-1.21680543282056,0.000145867497023454));
#8091=CARTESIAN_POINT('',(-1.25489265014994,-1.21681358531413,-0.000118566432341596));
#8092=CARTESIAN_POINT('',(-1.1,-1.215,-1.48794586096403E-16));
#8093=CARTESIAN_POINT('Ctrl Pts',(-1.19010734985006,-1.21680543282056,0.000145867497023454));
#8094=CARTESIAN_POINT('Ctrl Pts',(-1.19061068016911,-1.21682033874597,0.00864914984812415));
#8095=CARTESIAN_POINT('Ctrl Pts',(-1.19111401048817,-1.21673860976105,0.0171521385756626));
#8096=CARTESIAN_POINT('Ctrl Pts',(-1.19161734080722,-1.21655935421094,0.0256530708019106));
#8097=CARTESIAN_POINT('Ctrl Pts',(-1.2149823867054,-1.20823815042624,0.42027398697765));
#8098=CARTESIAN_POINT('Ctrl Pts',(-1.23834743260358,-0.989756964692678,
0.810463348804642));
#8099=CARTESIAN_POINT('Ctrl Pts',(-1.26171247850176,-0.657664591757992,
1.02379297304796));
#8100=CARTESIAN_POINT('Ctrl Pts',(-1.28507752439994,-0.325572218823306,
1.23712259729128));
#8101=CARTESIAN_POINT('Ctrl Pts',(-1.30844257029812,0.120131341312504,1.27359248395092));
#8102=CARTESIAN_POINT('Ctrl Pts',(-1.3318076161963,0.48248577096526,1.11708642885146));
#8103=CARTESIAN_POINT('Ctrl Pts',(-1.35517266209448,0.844840200618017,0.960580373751996));
#8104=CARTESIAN_POINT('Ctrl Pts',(-1.37853770799267,1.12384549978772,0.611098376893435));
#8105=CARTESIAN_POINT('Ctrl Pts',(-1.40190275389085,1.19620669325149,0.223079283185934));
#8106=CARTESIAN_POINT('Ctrl Pts',(-1.42526779978903,1.26856788671526,-0.164939810521567));
#8107=CARTESIAN_POINT('Ctrl Pts',(-1.44863284568721,1.13428497447309,-0.591496001078011));
#8108=CARTESIAN_POINT('Ctrl Pts',(-1.47199789158539,0.852698879583878,-0.868089649892069));
#8109=CARTESIAN_POINT('Ctrl Pts',(-1.49536293748357,0.571112784694665,-1.14468329870613));
#8110=CARTESIAN_POINT('Ctrl Pts',(-1.51872798338175,0.142223507158407,-1.2713144057778));
#8111=CARTESIAN_POINT('Ctrl Pts',(-1.54209302927993,-0.244439197279475,
-1.19202486410288));
#8112=CARTESIAN_POINT('Ctrl Pts',(-1.56545807517811,-0.631101901717355,
-1.11273532242796));
#8113=CARTESIAN_POINT('Ctrl Pts',(-1.58882312107629,-0.975538033056859,
-0.827525132006445));
#8114=CARTESIAN_POINT('Ctrl Pts',(-1.61218816697447,-1.12553780237062,-0.462428722136953));
#8115=CARTESIAN_POINT('Ctrl Pts',(-1.62149456126633,-1.18528333007065,-0.317009314034972));
#8116=CARTESIAN_POINT('Ctrl Pts',(-1.6308009555582,-1.21418227160102,-0.158916262349573));
#8117=CARTESIAN_POINT('Ctrl Pts',(-1.64010734985006,-1.21347552231432,-0.000575546447129233));
#8118=CARTESIAN_POINT('Ctrl Pts',(-1.70489265014994,-1.21328542726779,-0.000363737954992407));
#8119=CARTESIAN_POINT('Ctrl Pts',(-1.69467473291451,-1.21377857191844,-0.174284327370441));
#8120=CARTESIAN_POINT('Ctrl Pts',(-1.68445681567909,-1.17871053439215,-0.348016506489212));
#8121=CARTESIAN_POINT('Ctrl Pts',(-1.67423889844366,-1.10706686273875,-0.505060300998285));
#8122=CARTESIAN_POINT('Ctrl Pts',(-1.65087385254548,-0.943241139949365,
-0.864168266172182));
#8123=CARTESIAN_POINT('Ctrl Pts',(-1.6275088066473,-0.588165885554272,-1.1360147028441));
#8124=CARTESIAN_POINT('Ctrl Pts',(-1.60414376074912,-0.198757634157503,
-1.20048470038601));
#8125=CARTESIAN_POINT('Ctrl Pts',(-1.58077871485094,0.190650617239263,-1.26495469792792));
#8126=CARTESIAN_POINT('Ctrl Pts',(-1.55741366895276,0.614391865637705,-1.12204825633983));
#8127=CARTESIAN_POINT('Ctrl Pts',(-1.53404862305458,0.885214061026173,-0.834908355079327));
#8128=CARTESIAN_POINT('Ctrl Pts',(-1.5106835771564,1.15603625641464,-0.547768453818826));
#8129=CARTESIAN_POINT('Ctrl Pts',(-1.48731853125821,1.27393939879314,-0.11639509288592));
#8130=CARTESIAN_POINT('Ctrl Pts',(-1.46395348536003,1.18681948727553,0.268579473257125));
#8131=CARTESIAN_POINT('Ctrl Pts',(-1.44058843946185,1.09969957575793,0.653554039400168));
#8132=CARTESIAN_POINT('Ctrl Pts',(-1.41722339356367,0.807556610344237,0.992129810753349));
#8133=CARTESIAN_POINT('Ctrl Pts',(-1.39385834766549,0.439491974942901,1.13468954182857));
#8134=CARTESIAN_POINT('Ctrl Pts',(-1.37049330176731,0.0714273395415663,
1.27724927290379));
#8135=CARTESIAN_POINT('Ctrl Pts',(-1.34712825586913,-0.372558965847411,
1.22379296370105));
#8136=CARTESIAN_POINT('Ctrl Pts',(-1.32376320997095,-0.696265889399082,
0.997942178270234));
#8137=CARTESIAN_POINT('Ctrl Pts',(-1.30080635669728,-1.01431757994704,0.776037057027471));
#8138=CARTESIAN_POINT('Ctrl Pts',(-1.27784950342361,-1.21625579422078,0.387708384054187));
#8139=CARTESIAN_POINT('Ctrl Pts',(-1.25489265014994,-1.21681358531413,-0.000118566432341596));
#8140=CARTESIAN_POINT('Origin',(-1.1,0.,0.));
#8141=CARTESIAN_POINT('',(-0.74010734985006,-1.21327246620193,0.000345136923926501));
#8142=CARTESIAN_POINT('',(-0.804892650149939,-1.21345200008106,0.000555700457907037));
#8143=CARTESIAN_POINT('',(-1.1,-1.215,-1.48794586096403E-16));
#8144=CARTESIAN_POINT('Ctrl Pts',(-0.74010734985006,-1.21327246620193,0.000345136923926501));
#8145=CARTESIAN_POINT('Ctrl Pts',(-0.750420404780028,-1.21373773246957,
0.175887272582135));
#8146=CARTESIAN_POINT('Ctrl Pts',(-0.760733459709996,-1.17798633483971,
0.351249023172776));
#8147=CARTESIAN_POINT('Ctrl Pts',(-0.771046514639964,-1.10504391190561,
0.509464052100677));
#8148=CARTESIAN_POINT('Ctrl Pts',(-0.794411560538145,-0.939787053355631,
0.867912779251391));
#8149=CARTESIAN_POINT('Ctrl Pts',(-0.817776606436326,-0.583634221976302,
1.13834994754172));
#8150=CARTESIAN_POINT('Ctrl Pts',(-0.841141652334506,-0.193972815310299,
1.20126947215299));
#8151=CARTESIAN_POINT('Ctrl Pts',(-0.864506698232687,0.195688591355703,
1.26418899676426));
#8152=CARTESIAN_POINT('Ctrl Pts',(-0.887871744130868,0.618858573308381,
1.11959087769647));
#8153=CARTESIAN_POINT('Ctrl Pts',(-0.911236790029049,0.888534727151963,
0.831372995795705));
#8154=CARTESIAN_POINT('Ctrl Pts',(-0.93460183592723,1.15821088099554,0.54315511389494));
#8155=CARTESIAN_POINT('Ctrl Pts',(-0.957966881825411,1.27439320673003,0.111317469161196));
#8156=CARTESIAN_POINT('Ctrl Pts',(-0.981331927723592,1.18573961955721,-0.273306374200708));
#8157=CARTESIAN_POINT('Ctrl Pts',(-1.00469697362177,1.09708603238439,-0.657930217562613));
#8158=CARTESIAN_POINT('Ctrl Pts',(-1.02806201951995,0.803596532304258,-0.995340259552676));
#8159=CARTESIAN_POINT('Ctrl Pts',(-1.05142706541813,0.434966776615619,-1.13643236136105));
#8160=CARTESIAN_POINT('Ctrl Pts',(-1.07479211131631,0.0663370209269809,
-1.27752446316943));
#8161=CARTESIAN_POINT('Ctrl Pts',(-1.0981571572145,-0.377432990370165,-1.22229862479612));
#8162=CARTESIAN_POINT('Ctrl Pts',(-1.12152220311268,-0.70023738510082,-0.995159470347216));
#8163=CARTESIAN_POINT('Ctrl Pts',(-1.1443839186918,-1.016087920648,-0.772913352427169));
#8164=CARTESIAN_POINT('Ctrl Pts',(-1.16724563427093,-1.21612839228815,-0.386080861236012));
#8165=CARTESIAN_POINT('Ctrl Pts',(-1.19010734985006,-1.21680543282056,0.000145867497023454));
#8166=CARTESIAN_POINT('Ctrl Pts',(-1.25489265014994,-1.21681358531413,-0.000118566432341596));
#8167=CARTESIAN_POINT('Ctrl Pts',(-1.25448445752543,-1.2168235033202,-0.00701446365691278));
#8168=CARTESIAN_POINT('Ctrl Pts',(-1.25407626490092,-1.21676975308714,-0.0139102022573895));
#8169=CARTESIAN_POINT('Ctrl Pts',(-1.25366807227641,-1.21665185527998,-0.0208048438500122));
#8170=CARTESIAN_POINT('Ctrl Pts',(-1.23030302637823,-1.20990335589485,-0.415455818880555));
#8171=CARTESIAN_POINT('Ctrl Pts',(-1.20693798048005,-0.992978815410212,
-0.806512507282753));
#8172=CARTESIAN_POINT('Ctrl Pts',(-1.18357293458187,-0.661739228727891,
-1.02116382620166));
#8173=CARTESIAN_POINT('Ctrl Pts',(-1.16020788868369,-0.330499642045568,
-1.23581514512057));
#8174=CARTESIAN_POINT('Ctrl Pts',(-1.13684284278551,0.11505499083444,-1.27406109455618));
#8175=CARTESIAN_POINT('Ctrl Pts',(-1.11347779688732,0.47803019109439,-1.11900029591178));
#8176=CARTESIAN_POINT('Ctrl Pts',(-1.09011275098914,0.841005391354337,-0.963939497267381));
#8177=CARTESIAN_POINT('Ctrl Pts',(-1.06674770509096,1.12140115899423,-0.615571950542975));
#8178=CARTESIAN_POINT('Ctrl Pts',(-1.04338265919278,1.19530808939557,-0.227844404091649));
#8179=CARTESIAN_POINT('Ctrl Pts',(-1.0200176132946,1.26921501979691,0.159883142359683));
#8180=CARTESIAN_POINT('Ctrl Pts',(-0.996652567396421,1.1366331129597,0.586970688537935));
#8181=CARTESIAN_POINT('Ctrl Pts',(-0.97328752149824,0.856151500849342,0.864684412627987));
#8182=CARTESIAN_POINT('Ctrl Pts',(-0.949922475600059,0.575669888738987,
1.14239813671804));
#8183=CARTESIAN_POINT('Ctrl Pts',(-0.926557429701878,0.147288571355488,
1.27073803871989));
#8184=CARTESIAN_POINT('Ctrl Pts',(-0.903192383803698,-0.239686951572779,
1.19298974514702));
#8185=CARTESIAN_POINT('Ctrl Pts',(-0.879827337905517,-0.626662474501049,
1.11524145157414));
#8186=CARTESIAN_POINT('Ctrl Pts',(-0.856462292007336,-0.972232202974088,
0.831404962426542));
#8187=CARTESIAN_POINT('Ctrl Pts',(-0.833097246109155,-1.12368582435133,
0.466909784257848));
#8188=CARTESIAN_POINT('Ctrl Pts',(-0.82369571412275,-1.18462711554503,0.320245699309042));
#8189=CARTESIAN_POINT('Ctrl Pts',(-0.814294182136344,-1.21413976936114,
0.160522457515797));
#8190=CARTESIAN_POINT('Ctrl Pts',(-0.804892650149939,-1.21345200008106,
0.000555700457907037));
#8191=CARTESIAN_POINT('Origin',(-1.1,0.,0.));
#8192=CARTESIAN_POINT('',(-0.29010734985006,-1.21601418463372,-0.00087989446188777));
#8193=CARTESIAN_POINT('',(-0.354892650149939,-1.2156153315498,-0.000937869499410686));
#8194=CARTESIAN_POINT('',(-1.1,-1.215,-1.48794586096403E-16));
#8195=CARTESIAN_POINT('Ctrl Pts',(-0.29010734985006,-1.21601418463372,-0.00087989446188777));
#8196=CARTESIAN_POINT('Ctrl Pts',(-0.310230129390944,-1.21339239274019,
0.339644417133859));
#8197=CARTESIAN_POINT('Ctrl Pts',(-0.330352908931827,-1.06334626260878,
0.682304929774367));
#8198=CARTESIAN_POINT('Ctrl Pts',(-0.350475688472711,-0.809560818622168,
0.90849068695983));
#8199=CARTESIAN_POINT('Ctrl Pts',(-0.373840734370892,-0.514884403021141,
1.17112043884951));
#8200=CARTESIAN_POINT('Ctrl Pts',(-0.397205780269073,-0.0803456732840405,
1.27671783501035));
#8201=CARTESIAN_POINT('Ctrl Pts',(-0.420570826167254,0.302014387470901,
1.1787369191183));
#8202=CARTESIAN_POINT('Ctrl Pts',(-0.443935872065435,0.684374448225843,
1.08075600322626));
#8203=CARTESIAN_POINT('Ctrl Pts',(-0.467300917963614,1.01455583999862,0.779196775281337));
#8204=CARTESIAN_POINT('Ctrl Pts',(-0.490665963861795,1.14665608671571,0.407258679262273));
#8205=CARTESIAN_POINT('Ctrl Pts',(-0.514031009759976,1.27875633343279,0.0353205832432076));
#8206=CARTESIAN_POINT('Ctrl Pts',(-0.537396055658157,1.21277543509418,-0.406996380850001));
#8207=CARTESIAN_POINT('Ctrl Pts',(-0.560761101556338,0.977866936696777,
-0.724195707500305));
#8208=CARTESIAN_POINT('Ctrl Pts',(-0.584126147454519,0.74295843829938,-1.04139503415061));
#8209=CARTESIAN_POINT('Ctrl Pts',(-0.6074911933527,0.339122339843202,-1.23347672335801));
#8210=CARTESIAN_POINT('Ctrl Pts',(-0.63085623925088,-0.0551805065988665,
-1.21557537371284));
#8211=CARTESIAN_POINT('Ctrl Pts',(-0.654221285149061,-0.449483353040935,
-1.19767402406768));
#8212=CARTESIAN_POINT('Ctrl Pts',(-0.677586331047242,-0.834252947468894,
-0.969789635569952));
#8213=CARTESIAN_POINT('Ctrl Pts',(-0.700951376945423,-1.03945730182256,
-0.632617298315537));
#8214=CARTESIAN_POINT('Ctrl Pts',(-0.714003367913635,-1.15408688103817,
-0.444268843116553));
#8215=CARTESIAN_POINT('Ctrl Pts',(-0.727055358881848,-1.21268363474857,
-0.221817392482749));
#8216=CARTESIAN_POINT('Ctrl Pts',(-0.74010734985006,-1.21327246620193,0.000345136923926501));
#8217=CARTESIAN_POINT('Ctrl Pts',(-0.804892650149939,-1.21345200008106,
0.000555700457907037));
#8218=CARTESIAN_POINT('Ctrl Pts',(-0.790929136238163,-1.21243049891249,
-0.237033028786364));
#8219=CARTESIAN_POINT('Ctrl Pts',(-0.776965622326388,-1.14478890768345,
-0.475158936228772));
#8220=CARTESIAN_POINT('Ctrl Pts',(-0.763002108414612,-1.01455126765528,
-0.671833688654041));
#8221=CARTESIAN_POINT('Ctrl Pts',(-0.739637062516432,-0.796625575300528,
-1.00092811620745));
#8222=CARTESIAN_POINT('Ctrl Pts',(-0.716272016618252,-0.403436676309569,
-1.21396310412447));
#8223=CARTESIAN_POINT('Ctrl Pts',(-0.692906970720071,-0.00873828951562631,
-1.21679792680243));
#8224=CARTESIAN_POINT('Ctrl Pts',(-0.66954192482189,0.385960097278319,-1.21963274948038));
#8225=CARTESIAN_POINT('Ctrl Pts',(-0.646176878923709,0.782167971875248,
-1.01226740691925));
#8226=CARTESIAN_POINT('Ctrl Pts',(-0.622811833025528,1.00479768075463,-0.686335959703516));
#8227=CARTESIAN_POINT('Ctrl Pts',(-0.599446787127348,1.22742738963402,-0.360404512487788));
#8228=CARTESIAN_POINT('Ctrl Pts',(-0.576081741229167,1.27647893279586,0.0840930393825391));
#8229=CARTESIAN_POINT('Ctrl Pts',(-0.552716695330987,1.13027577545516,0.450724490835534));
#8230=CARTESIAN_POINT('Ctrl Pts',(-0.529351649432806,0.984072618114463,
0.817355942288532));
#8231=CARTESIAN_POINT('Ctrl Pts',(-0.505986603534625,0.642614760271223,
1.1061212933242));
#8232=CARTESIAN_POINT('Ctrl Pts',(-0.482621557636444,0.256795879861456,
1.18942170363709));
#8233=CARTESIAN_POINT('Ctrl Pts',(-0.459256511738263,-0.129023000548309,
1.27272211394999));
#8234=CARTESIAN_POINT('Ctrl Pts',(-0.435891465840083,-0.559202903524601,
1.15055758354011));
#8235=CARTESIAN_POINT('Ctrl Pts',(-0.412526419941902,-0.84364432694555,
0.876896342694676));
#8236=CARTESIAN_POINT('Ctrl Pts',(-0.393315163344581,-1.07751834525735,
0.651886028504265));
#8237=CARTESIAN_POINT('Ctrl Pts',(-0.37410390674726,-1.21286598892674,0.324456492602413));
#8238=CARTESIAN_POINT('Ctrl Pts',(-0.354892650149939,-1.2156153315498,-0.000937869499410686));
#8239=CARTESIAN_POINT('Origin',(-3.06687266823562,0.,0.));
#8240=CARTESIAN_POINT('',(-0.141872668235622,-0.959049870308857,-0.000693957916149163));
#8241=CARTESIAN_POINT('',(-0.0531273317643739,-0.958113697008845,0.00104402191651295));
#8242=CARTESIAN_POINT('',(-3.06687266823562,-0.95825,-2.57321451159241E-15));
#8243=CARTESIAN_POINT('',(5.20417042793042E-17,0.382997178453078,-0.879688698994096));
#8244=CARTESIAN_POINT('Ctrl Pts',(-0.141872668235623,-0.959049870308857,
-0.000693957916149159));
#8245=CARTESIAN_POINT('Ctrl Pts',(-0.138630401878326,-0.959383036932027,
-0.0439663989064678));
#8246=CARTESIAN_POINT('Ctrl Pts',(-0.112023089622848,-0.937346021668143,
-0.398718122803486));
#8247=CARTESIAN_POINT('Ctrl Pts',(-0.064732200210974,-0.519622583613204,
-0.977168669190065));
#8248=CARTESIAN_POINT('Ctrl Pts',(-0.0206835771563966,0.129196057750057,
-0.988008553242574));
#8249=CARTESIAN_POINT('Ctrl Pts',(1.95156391047391E-17,0.382997178453079,
-0.879688698994096));
#8250=CARTESIAN_POINT('',(0.,-0.706474930361996,-0.647407317899646));
#8251=CARTESIAN_POINT('Origin',(0.,0.,0.));
#8252=CARTESIAN_POINT('Ctrl Pts',(-0.0531273317643739,-0.958113697008845,
0.00104402191651295));
#8253=CARTESIAN_POINT('Ctrl Pts',(-0.0354182211762492,-0.955989012569265,
-0.235236130484369));
#8254=CARTESIAN_POINT('Ctrl Pts',(-0.0177091105881247,-0.866556638099344,
-0.47272020794717));
#8255=CARTESIAN_POINT('Ctrl Pts',(0.,-0.706474930361996,-0.647407317899646));
#8256=CARTESIAN_POINT('Origin',(-3.06687266823562,0.,0.));
#8257=CARTESIAN_POINT('',(-0.591872668235624,-0.956887523241153,0.000272203668602481));
#8258=CARTESIAN_POINT('',(-0.503127331764375,-0.958735301611192,-0.00073968185005005));
#8259=CARTESIAN_POINT('',(-3.06687266823562,-0.95825,-2.57321451159241E-15));
#8260=CARTESIAN_POINT('Ctrl Pts',(-0.591872668235624,-0.956887523241153,
0.000272203668602485));
#8261=CARTESIAN_POINT('Ctrl Pts',(-0.578820677267412,-0.956423121808899,
-0.174943634853164));
#8262=CARTESIAN_POINT('Ctrl Pts',(-0.542403640401018,-0.827478287706606,
-0.664458216830761));
#8263=CARTESIAN_POINT('Ctrl Pts',(-0.482621557636444,-0.0510386495398221,
-1.12431386735868));
#8264=CARTESIAN_POINT('Ctrl Pts',(-0.412526419941902,0.904457501930876,
-0.669839105178461));
#8265=CARTESIAN_POINT('Ctrl Pts',(-0.342431282247359,1.06057156571601,0.37670467467911));
#8266=CARTESIAN_POINT('Ctrl Pts',(-0.272336144552818,0.279346087527691,
1.09020869981052));
#8267=CARTESIAN_POINT('Ctrl Pts',(-0.205483273215571,-0.701237154507542,
0.85191685148548));
#8268=CARTESIAN_POINT('Ctrl Pts',(-0.161995447776507,-0.956982107278429,
0.267871821167497));
#8269=CARTESIAN_POINT('Ctrl Pts',(-0.141872668235623,-0.959049870308857,
-0.000693957916149159));
#8270=CARTESIAN_POINT('Ctrl Pts',(-0.503127331764375,-0.958735301611192,
-0.000739681850050059));
#8271=CARTESIAN_POINT('Ctrl Pts',(-0.498973542463515,-0.959204136697488,
-0.0562279620506522));
#8272=CARTESIAN_POINT('Ctrl Pts',(-0.471454707264475,-0.929920724358644,
-0.423340439029663));
#8273=CARTESIAN_POINT('Ctrl Pts',(-0.420570826167254,-0.456959852937158,
-1.02848258701033));
#8274=CARTESIAN_POINT('Ctrl Pts',(-0.350475688472711,0.598427973773188,
-0.953300309276372));
#8275=CARTESIAN_POINT('Ctrl Pts',(-0.280380550778169,1.12493185591355,-0.0352038077644344));
#8276=CARTESIAN_POINT('Ctrl Pts',(-0.210285413083627,0.657167771359294,
0.913300215389848));
#8277=CARTESIAN_POINT('Ctrl Pts',(-0.140190275389085,-0.391346585807462,
1.05597004801595));
#8278=CARTESIAN_POINT('Ctrl Pts',(-0.0878042482826666,-0.916578406566786,
0.46308350348097));
#8279=CARTESIAN_POINT('Ctrl Pts',(-0.0587832670744299,-0.958792278673619,
0.0765071712587342));
#8280=CARTESIAN_POINT('Ctrl Pts',(-0.0531273317643739,-0.958113697008845,
0.00104402191651295));
#8281=CARTESIAN_POINT('Origin',(-3.06687266823562,0.,0.));
#8282=CARTESIAN_POINT('',(-1.04187266823562,-0.959673914403541,0.000115043233756074));
#8283=CARTESIAN_POINT('',(-0.953127331764375,-0.957029118582447,0.000438271575131308));
#8284=CARTESIAN_POINT('',(-3.06687266823562,-0.95825,-2.57321451159241E-15));
#8285=CARTESIAN_POINT('Ctrl Pts',(-1.04187266823562,-0.959673914403541,
0.000115043233756108));
#8286=CARTESIAN_POINT('Ctrl Pts',(-1.0190109526565,-0.959139943958945,-0.304495461135321));
#8287=CARTESIAN_POINT('Ctrl Pts',(-0.972784191179187,-0.640129375198145,
-0.921388892840649));
#8288=CARTESIAN_POINT('Ctrl Pts',(-0.903192383803697,0.402312809571003,
-1.05111767609328));
#8289=CARTESIAN_POINT('Ctrl Pts',(-0.833097246109155,1.09672346006924,-0.252788854520488));
#8290=CARTESIAN_POINT('Ctrl Pts',(-0.763002108414613,0.821830339982639,
0.76896033823534));
#8291=CARTESIAN_POINT('Ctrl Pts',(-0.69290697072007,-0.17941073460045,1.11108662859757));
#8292=CARTESIAN_POINT('Ctrl Pts',(-0.635863823993741,-0.86517647964954,
0.59036482081822));
#8293=CARTESIAN_POINT('Ctrl Pts',(-0.602185723165592,-0.95725447089627,
0.138719324240192));
#8294=CARTESIAN_POINT('Ctrl Pts',(-0.591872668235624,-0.956887523241153,
0.000272203668602485));
#8295=CARTESIAN_POINT('Ctrl Pts',(-0.953127331764375,-0.957029118582447,
0.00043827157513129));
#8296=CARTESIAN_POINT('Ctrl Pts',(-0.9391638178526,-0.956223477846001,-0.1869439504811));
#8297=CARTESIAN_POINT('Ctrl Pts',(-0.901835258042643,-0.813609242388342,
-0.689004053082304));
#8298=CARTESIAN_POINT('Ctrl Pts',(-0.841141652334508,-0.00808224906629952,
-1.12544931827059));
#8299=CARTESIAN_POINT('Ctrl Pts',(-0.771046514639964,0.929365148050997,
-0.634812677507132));
#8300=CARTESIAN_POINT('Ctrl Pts',(-0.700951376945424,1.04542352147034,0.416890480714455));
#8301=CARTESIAN_POINT('Ctrl Pts',(-0.630856239250879,0.237517367696804,
1.10012356128217));
#8302=CARTESIAN_POINT('Ctrl Pts',(-0.564914890857198,-0.719993809571971,
0.828204992971714));
#8303=CARTESIAN_POINT('Ctrl Pts',(-0.522338588361696,-0.956566941472467,
0.255893361346717));
#8304=CARTESIAN_POINT('Ctrl Pts',(-0.503127331764375,-0.958735301611192,
-0.000739681850050059));
#8305=CARTESIAN_POINT('Origin',(-3.06687266823562,0.,0.));
#8306=CARTESIAN_POINT('',(-1.49187266823562,-0.957047670170947,-0.000453923771978915));
#8307=CARTESIAN_POINT('',(-1.40312733176438,-0.959680344137663,-9.35113446810798E-5));
#8308=CARTESIAN_POINT('',(-3.06687266823562,-0.95825,-2.57321451159241E-15));
#8309=CARTESIAN_POINT('Ctrl Pts',(-1.49187266823562,-0.957047670170947,
-0.000453923771978936));
#8310=CARTESIAN_POINT('Ctrl Pts',(-1.48256627394376,-0.957605071408786,
-0.125334574811913));
#8311=CARTESIAN_POINT('Ctrl Pts',(-1.44989483375372,-0.877590088530535,
-0.563060392917903));
#8312=CARTESIAN_POINT('Ctrl Pts',(-1.39385834766549,-0.226088456349441,
-1.10253603924939));
#8313=CARTESIAN_POINT('Ctrl Pts',(-1.32376320997095,0.788684754018751,-0.802920586529807));
#8314=CARTESIAN_POINT('Ctrl Pts',(-1.25366807227641,1.10640475563864,0.206332424829975));
#8315=CARTESIAN_POINT('Ctrl Pts',(-1.18357293458187,0.446264439763658,1.03322408776754));
#8316=CARTESIAN_POINT('Ctrl Pts',(-1.11347779688732,-0.608292193570018,
0.946934534948777));
#8317=CARTESIAN_POINT('Ctrl Pts',(-1.06624437477191,-0.956629001276476,
0.324833752021017));
#8318=CARTESIAN_POINT('Ctrl Pts',(-1.04237599855468,-0.959685670455414,
0.00682143855305239));
#8319=CARTESIAN_POINT('Ctrl Pts',(-1.04187266823562,-0.959673914403541,
0.000115043233756108));
#8320=CARTESIAN_POINT('Ctrl Pts',(-1.40312733176438,-0.959680344137663,
-9.35113446812153E-5));
#8321=CARTESIAN_POINT('Ctrl Pts',(-1.40271913913987,-0.959688166301716,
-0.00553218913517348));
#8322=CARTESIAN_POINT('Ctrl Pts',(-1.37894590061717,-0.957219251541219,
-0.3222748308864));
#8323=CARTESIAN_POINT('Ctrl Pts',(-1.3318076161963,-0.612060912713934,-0.944502618736714));
#8324=CARTESIAN_POINT('Ctrl Pts',(-1.26171247850176,0.44214335137808,-1.03499442379023));
#8325=CARTESIAN_POINT('Ctrl Pts',(-1.19161734080722,1.10557358431864,-0.210739604904639));
#8326=CARTESIAN_POINT('Ctrl Pts',(-1.12152220311268,0.791878245487139,0.799770620096117));
#8327=CARTESIAN_POINT('Ctrl Pts',(-1.05142706541813,-0.22169310607518,1.10342916600544));
#8328=CARTESIAN_POINT('Ctrl Pts',(-0.995295441635367,-0.876448687134617,
0.565640378200179));
#8329=CARTESIAN_POINT('Ctrl Pts',(-0.962528863750781,-0.957571550609307,
0.126601353839102));
#8330=CARTESIAN_POINT('Ctrl Pts',(-0.953127331764375,-0.957029118582447,
0.00043827157513129));
#8331=CARTESIAN_POINT('Origin',(-3.06687266823562,0.,0.));
#8332=CARTESIAN_POINT('',(-1.94187266823562,-0.958689328197825,0.000800959330899789));
#8333=CARTESIAN_POINT('',(-1.85312733176438,-0.956897745415108,-0.00028687398796072));
#8334=CARTESIAN_POINT('',(-3.06687266823562,-0.95825,-2.57321451159241E-15));
#8335=CARTESIAN_POINT('Ctrl Pts',(-1.94187266823562,-0.958689328197825,
0.000800959330899747));
#8336=CARTESIAN_POINT('Ctrl Pts',(-1.92275654933285,-0.956519486288093,
-0.254585784224982));
#8337=CARTESIAN_POINT('Ctrl Pts',(-1.88027538453189,-0.721924785019282,
-0.825806756370372));
#8338=CARTESIAN_POINT('Ctrl Pts',(-1.81442917383274,0.233140677181374,-1.1010152907217));
#8339=CARTESIAN_POINT('Ctrl Pts',(-1.74433403613821,1.04374906965657,-0.421077590856424));
#8340=CARTESIAN_POINT('Ctrl Pts',(-1.67423889844366,0.931890207415111,0.631116820366198));
#8341=CARTESIAN_POINT('Ctrl Pts',(-1.60414376074912,-0.00359849674038535,
1.12546597767462));
#8342=CARTESIAN_POINT('Ctrl Pts',(-1.54335501734644,-0.812122043604567,
0.691564032716878));
#8343=CARTESIAN_POINT('Ctrl Pts',(-1.50593131984194,-0.956205635161259,
0.188196321455179));
#8344=CARTESIAN_POINT('Ctrl Pts',(-1.49187266823562,-0.957047670170947,
-0.000453923771978936));
#8345=CARTESIAN_POINT('Ctrl Pts',(-1.85312733176438,-0.956897745415108,
-0.000286873987960694));
#8346=CARTESIAN_POINT('Ctrl Pts',(-1.84290941452895,-0.957286680280528,
-0.137455108397305));
#8347=CARTESIAN_POINT('Ctrl Pts',(-1.80932645139534,-0.866385265055213,
-0.587793994348256));
#8348=CARTESIAN_POINT('Ctrl Pts',(-1.75237844236356,-0.183834647990358,
-1.1103563267006));
#8349=CARTESIAN_POINT('Ctrl Pts',(-1.68228330466901,0.818758071214107,-0.772232628794933));
#8350=CARTESIAN_POINT('Ctrl Pts',(-1.61218816697447,1.09772272845902,0.248418045560514));
#8351=CARTESIAN_POINT('Ctrl Pts',(-1.54209302927993,0.406498045477112,1.04950504037332));
#8352=CARTESIAN_POINT('Ctrl Pts',(-1.4724060842099,-0.637878025349449,0.923761319253053));
#8353=CARTESIAN_POINT('Ctrl Pts',(-1.42608418503805,-0.959240423713628,
0.30577906092175));
#8354=CARTESIAN_POINT('Ctrl Pts',(-1.40312733176438,-0.959680344137663,
-9.35113446812153E-5));
#8355=CARTESIAN_POINT('Ctrl Pts',(-2.38323468161444,-0.418777734803984,
0.861898063191027));
#8356=CARTESIAN_POINT('Ctrl Pts',(-2.35986963571626,-0.699961277147284,
0.725277026486611));
#8357=CARTESIAN_POINT('Ctrl Pts',(-2.3131395439199,-1.11403436160083,0.158253196261579));
#8358=CARTESIAN_POINT('Ctrl Pts',(-2.24304440622535,-0.752359592709721,
-0.837961774657783));
#8359=CARTESIAN_POINT('Ctrl Pts',(-2.17294926853081,0.275115309926484,-1.09100794194568));
#8360=CARTESIAN_POINT('Ctrl Pts',(-2.10285413083626,1.05900093864512,-0.381087916994184));
#8361=CARTESIAN_POINT('Ctrl Pts',(-2.03275899314173,0.907151642232085,0.666313302776059));
#8362=CARTESIAN_POINT('Ctrl Pts',(-1.96266385544718,-0.0465745614418721,
1.12446411646007));
#8363=CARTESIAN_POINT('Ctrl Pts',(-1.89256871775265,-0.959074148548053,
0.588978031955627));
#8364=CARTESIAN_POINT('Ctrl Pts',(-1.8224735800581,-1.02396023446961,-0.467154233019447));
#8365=CARTESIAN_POINT('Ctrl Pts',(-1.75237844236356,-0.183834647990358,
-1.1103563267006));
#8366=CARTESIAN_POINT('Ctrl Pts',(-1.68228330466901,0.818758071214107,-0.772232628794933));
#8367=CARTESIAN_POINT('Ctrl Pts',(-1.61218816697447,1.09772272845902,0.248418045560514));
#8368=CARTESIAN_POINT('Ctrl Pts',(-1.54209302927993,0.406498045477112,1.04950504037332));
#8369=CARTESIAN_POINT('Ctrl Pts',(-1.47199789158539,-0.643995478322856,
0.923024772981895));
#8370=CARTESIAN_POINT('Ctrl Pts',(-1.40190275389085,-1.12531508782357,-0.0192431825357103));
#8371=CARTESIAN_POINT('Ctrl Pts',(-1.3318076161963,-0.612060912713934,-0.944502618736714));
#8372=CARTESIAN_POINT('Ctrl Pts',(-1.26171247850176,0.44214335137808,-1.03499442379023));
#8373=CARTESIAN_POINT('Ctrl Pts',(-1.19161734080722,1.10557358431864,-0.210739604904639));
#8374=CARTESIAN_POINT('Ctrl Pts',(-1.12152220311268,0.791878245487139,0.799770620096117));
#8375=CARTESIAN_POINT('Ctrl Pts',(-1.05142706541813,-0.22169310607518,1.10342916600544));
#8376=CARTESIAN_POINT('Ctrl Pts',(-0.981331927723592,-1.03932814881416,
0.431858016065468));
#8377=CARTESIAN_POINT('Ctrl Pts',(-0.911236790029049,-0.938386600814667,
-0.621398016612586));
#8378=CARTESIAN_POINT('Ctrl Pts',(-0.841141652334508,-0.00808224906629952,
-1.12544931827059));
#8379=CARTESIAN_POINT('Ctrl Pts',(-0.771046514639964,0.929365148050997,
-0.634812677507132));
#8380=CARTESIAN_POINT('Ctrl Pts',(-0.700951376945424,1.04542352147034,0.416890480714455));
#8381=CARTESIAN_POINT('Ctrl Pts',(-0.630856239250879,0.237517367696804,
1.10012356128217));
#8382=CARTESIAN_POINT('Ctrl Pts',(-0.560761101556339,-0.780309526197106,
0.811076249516093));
#8383=CARTESIAN_POINT('Ctrl Pts',(-0.490665963861796,-1.10848754091122,
-0.194868458669156));
#8384=CARTESIAN_POINT('Ctrl Pts',(-0.420570826167254,-0.456959852937158,
-1.02848258701033));
#8385=CARTESIAN_POINT('Ctrl Pts',(-0.350475688472711,0.598427973773188,
-0.953300309276372));
#8386=CARTESIAN_POINT('Ctrl Pts',(-0.280380550778169,1.12493185591355,-0.0352038077644344));
#8387=CARTESIAN_POINT('Ctrl Pts',(-0.210285413083627,0.657167771359294,
0.913300215389848));
#8388=CARTESIAN_POINT('Ctrl Pts',(-0.140190275389085,-0.391346585807462,
1.05597004801595));
#8389=CARTESIAN_POINT('Ctrl Pts',(-0.0700951376945419,-1.09413316519229,
0.262658047241422));
#8390=CARTESIAN_POINT('Ctrl Pts',(-0.0233650458981807,-0.917683530033312,
-0.416928643008026));
#8391=CARTESIAN_POINT('Ctrl Pts',(0.,-0.706474930361996,-0.647407317899646));
#8392=CARTESIAN_POINT('Ctrl Pts',(-2.33382312107629,-0.456179659636029,
0.938876001350623));
#8393=CARTESIAN_POINT('Ctrl Pts',(-2.31045807517811,-0.762476298595258,
0.790053051028027));
#8394=CARTESIAN_POINT('Ctrl Pts',(-2.26372798338175,-1.21353112561197,0.172387123782289));
#8395=CARTESIAN_POINT('Ctrl Pts',(-2.19363284568721,-0.819554418495693,
-0.912801912284841));
#8396=CARTESIAN_POINT('Ctrl Pts',(-2.12353770799266,0.299686439876436,-1.18844816773733));
#8397=CARTESIAN_POINT('Ctrl Pts',(-2.05344257029812,1.15358255130609,-0.415123684517711));
#8398=CARTESIAN_POINT('Ctrl Pts',(-1.98334743260358,0.988171273206288,0.725823152497863));
#8399=CARTESIAN_POINT('Ctrl Pts',(-1.91325229490904,-0.0507342339873809,
1.22489238392719));
#8400=CARTESIAN_POINT('Ctrl Pts',(-1.84315715721449,-1.04473108833054,0.641580905146204));
#8401=CARTESIAN_POINT('Ctrl Pts',(-1.77306201951995,-1.11541228776122,-0.50887676517972));
#8402=CARTESIAN_POINT('Ctrl Pts',(-1.70296688182541,-0.200253309046633,
-1.20952459763907));
#8403=CARTESIAN_POINT('Ctrl Pts',(-1.63287174413087,0.891883085488123,-0.841202357447199));
#8404=CARTESIAN_POINT('Ctrl Pts',(-1.56277660643633,1.19576266602989,0.270604786389338));
#8405=CARTESIAN_POINT('Ctrl Pts',(-1.49268146874178,0.442803245294923,1.14323855428439));
#8406=CARTESIAN_POINT('Ctrl Pts',(-1.42258633104724,-0.701512075960701,
1.0054620668207));
#8407=CARTESIAN_POINT('Ctrl Pts',(-1.3524911933527,-1.22581935734221,-0.0209618318499275));
#8408=CARTESIAN_POINT('Ctrl Pts',(-1.28239605565816,-0.66672536678448,-1.02885814438612));
#8409=CARTESIAN_POINT('Ctrl Pts',(-1.21230091796362,0.481632108823535,-1.12743196385742));
#8410=CARTESIAN_POINT('Ctrl Pts',(-1.14220578026907,1.2043146984238,-0.229561204542612));
#8411=CARTESIAN_POINT('Ctrl Pts',(-1.07211064257453,0.862602565698921,0.871199824969472));
#8412=CARTESIAN_POINT('Ctrl Pts',(-1.00201550487999,-0.241492986059457,
1.20197875757754));
#8413=CARTESIAN_POINT('Ctrl Pts',(-0.931920367185445,-1.13215274302515,
0.470428168469959));
#8414=CARTESIAN_POINT('Ctrl Pts',(-0.861825229490904,-1.02219589197361,
-0.676896387171863));
#8415=CARTESIAN_POINT('Ctrl Pts',(-0.791730091796362,-0.00880409181707018,
-1.22596557619423));
#8416=CARTESIAN_POINT('Ctrl Pts',(-0.721634954101819,1.01236871419139,-0.691509139790793));
#8417=CARTESIAN_POINT('Ctrl Pts',(-0.651539816407278,1.13879250629946,0.454123850893925));
#8418=CARTESIAN_POINT('Ctrl Pts',(-0.581444678712735,0.258730545940533,
1.19837792230807));
#8419=CARTESIAN_POINT('Ctrl Pts',(-0.511349541018193,-0.850000619631704,
0.883515184054141));
#8420=CARTESIAN_POINT('Ctrl Pts',(-0.44125440332365,-1.20748890664005,-0.212272572683697));
#8421=CARTESIAN_POINT('Ctrl Pts',(-0.371159265629109,-0.497771903460376,
-1.12033854116805));
#8422=CARTESIAN_POINT('Ctrl Pts',(-0.301064127934566,0.651874841245582,
-1.03844157526705));
#8423=CARTESIAN_POINT('Ctrl Pts',(-0.230968990240023,1.22540189818011,-0.0383479342601363));
#8424=CARTESIAN_POINT('Ctrl Pts',(-0.160873852545481,0.715860814335727,
0.994868988431449));
#8425=CARTESIAN_POINT('Ctrl Pts',(-0.090778714850939,-0.426298576730522,
1.15028096542724));
#8426=CARTESIAN_POINT('Ctrl Pts',(-0.0206835771563966,-1.19185251127912,
0.286116592725112));
#8427=CARTESIAN_POINT('Ctrl Pts',(0.0260465146399647,-0.999643786172473,
-0.454165421542616));
#8428=CARTESIAN_POINT('Ctrl Pts',(0.0494115605381454,-0.769571699949071,
-0.705228634143052));
#8429=CARTESIAN_POINT('Ctrl Pts',(-2.28441156053815,-0.493581584468075,
1.01585393951022));
#8430=CARTESIAN_POINT('Ctrl Pts',(-2.26104651463996,-0.824991320043233,
0.854829075569444));
#8431=CARTESIAN_POINT('Ctrl Pts',(-2.21431642284361,-1.3130278896231,0.186521051302999));
#8432=CARTESIAN_POINT('Ctrl Pts',(-2.14422128514906,-0.886749244281665,
-0.987642049911899));
#8433=CARTESIAN_POINT('Ctrl Pts',(-2.07412614745452,0.324257569826388,-1.28588839352898));
#8434=CARTESIAN_POINT('Ctrl Pts',(-2.00403100975997,1.24816416396707,-0.449159452041237));
#8435=CARTESIAN_POINT('Ctrl Pts',(-1.93393587206544,1.06919090418049,0.785333002219665));
#8436=CARTESIAN_POINT('Ctrl Pts',(-1.86384073437089,-0.0548939065328899,
1.32532065139432));
#8437=CARTESIAN_POINT('Ctrl Pts',(-1.79374559667635,-1.13038802811303,0.694183778336778));
#8438=CARTESIAN_POINT('Ctrl Pts',(-1.7236504589818,-1.20686434105284,-0.550599297339992));
#8439=CARTESIAN_POINT('Ctrl Pts',(-1.65355532128727,-0.216671970102907,
-1.30869286857755));
#8440=CARTESIAN_POINT('Ctrl Pts',(-1.58346018359272,0.965008099762136,-0.910172086099464));
#8441=CARTESIAN_POINT('Ctrl Pts',(-1.51336504589818,1.29380260360076,0.292791527218161));
#8442=CARTESIAN_POINT('Ctrl Pts',(-1.44326990820364,0.479108445112733,1.23697206819546));
#8443=CARTESIAN_POINT('Ctrl Pts',(-1.3731747705091,-0.759028673598546,1.0878993606595));
#8444=CARTESIAN_POINT('Ctrl Pts',(-1.30307963281456,-1.32632362686085,-0.0226804811641433));
#8445=CARTESIAN_POINT('Ctrl Pts',(-1.23298449512001,-0.721389820855027,
-1.11321367003554));
#8446=CARTESIAN_POINT('Ctrl Pts',(-1.16288935742547,0.52112086626899,-1.21986950392461));
#8447=CARTESIAN_POINT('Ctrl Pts',(-1.09279421973093,1.30305581252896,-0.248382804180586));
#8448=CARTESIAN_POINT('Ctrl Pts',(-1.02269908203639,0.933326885910705,0.942629029842827));
#8449=CARTESIAN_POINT('Ctrl Pts',(-0.952603944341841,-0.261292866043736,
1.30052834914964));
#8450=CARTESIAN_POINT('Ctrl Pts',(-0.882508806647302,-1.22497733723614,
0.50899832087445));
#8451=CARTESIAN_POINT('Ctrl Pts',(-0.812413668952757,-1.10600518313255,
-0.73239475773114));
#8452=CARTESIAN_POINT('Ctrl Pts',(-0.742318531258218,-0.00952593456783798,
-1.32648183411787));
#8453=CARTESIAN_POINT('Ctrl Pts',(-0.672223393563673,1.09537228033178,-0.748205602074454));
#8454=CARTESIAN_POINT('Ctrl Pts',(-0.602128255869133,1.23216149112858,0.491357221073396));
#8455=CARTESIAN_POINT('Ctrl Pts',(-0.532033118174589,0.27994372418426,1.29663228333396));
#8456=CARTESIAN_POINT('Ctrl Pts',(-0.461937980480048,-0.919691713066301,
0.955954118592191));
#8457=CARTESIAN_POINT('Ctrl Pts',(-0.391842842785505,-1.30649027236888,
-0.22967668669824));
#8458=CARTESIAN_POINT('Ctrl Pts',(-0.321747705090963,-0.538583953983592,
-1.21219449532577));
#8459=CARTESIAN_POINT('Ctrl Pts',(-0.251652567396421,0.705321708717977,
-1.12358284125773));
#8460=CARTESIAN_POINT('Ctrl Pts',(-0.181557429701878,1.32587194044667,-0.041492060755839));
#8461=CARTESIAN_POINT('Ctrl Pts',(-0.111462292007336,0.774553857312159,
1.07643776147305));
#8462=CARTESIAN_POINT('Ctrl Pts',(-0.0413671543127934,-0.461250567653581,
1.24459188283852));
#8463=CARTESIAN_POINT('Ctrl Pts',(0.0287279833817485,-1.28957185736595,
0.309575138208801));
#8464=CARTESIAN_POINT('Ctrl Pts',(0.0754580751781104,-1.08160404231163,
-0.491402200077204));
#8465=CARTESIAN_POINT('Ctrl Pts',(0.098823121076291,-0.832668469536145,
-0.763049950386459));
#8466=CARTESIAN_POINT('Ctrl Pts',(-2.235,-0.53098350930012,1.09283187766981));
#8467=CARTESIAN_POINT('Ctrl Pts',(-2.21163495410182,-0.887506341491207,
0.919605100110861));
#8468=CARTESIAN_POINT('Ctrl Pts',(-2.16490486230546,-1.41252465363424,0.200654978823709));
#8469=CARTESIAN_POINT('Ctrl Pts',(-2.09480972461092,-0.953944070067637,
-1.06248218753896));
#8470=CARTESIAN_POINT('Ctrl Pts',(-2.02471458691637,0.34882869977634,-1.38332861932063));
#8471=CARTESIAN_POINT('Ctrl Pts',(-1.95461944922183,1.34274577662804,-0.483195219564764));
#8472=CARTESIAN_POINT('Ctrl Pts',(-1.88452431152729,1.15021053515469,0.844842851941468));
#8473=CARTESIAN_POINT('Ctrl Pts',(-1.81442917383275,-0.0590535790783977,
1.42574891886144));
#8474=CARTESIAN_POINT('Ctrl Pts',(-1.7443340361382,-1.21604496789552,0.746786651527355));
#8475=CARTESIAN_POINT('Ctrl Pts',(-1.67423889844366,-1.29831639434446,-0.592321829500264));
#8476=CARTESIAN_POINT('Ctrl Pts',(-1.60414376074912,-0.233090631159182,
-1.40786113951602));
#8477=CARTESIAN_POINT('Ctrl Pts',(-1.53404862305458,1.03813311403615,-0.979141814751728));
#8478=CARTESIAN_POINT('Ctrl Pts',(-1.46395348536003,1.39184254117163,0.314978268046985));
#8479=CARTESIAN_POINT('Ctrl Pts',(-1.3938583476655,0.515413644930542,1.33070558210653));
#8480=CARTESIAN_POINT('Ctrl Pts',(-1.32376320997095,-0.816545271236388,
1.17033665449831));
#8481=CARTESIAN_POINT('Ctrl Pts',(-1.25366807227641,-1.42682789637949,-0.0243991304783595));
#8482=CARTESIAN_POINT('Ctrl Pts',(-1.18357293458187,-0.776054274925573,
-1.19756919568495));
#8483=CARTESIAN_POINT('Ctrl Pts',(-1.11347779688733,0.560609623714444,-1.31230704399179));
#8484=CARTESIAN_POINT('Ctrl Pts',(-1.04338265919278,1.40179692663412,-0.267204403818561));
#8485=CARTESIAN_POINT('Ctrl Pts',(-0.97328752149824,1.00405120612249,1.01405823471618));
#8486=CARTESIAN_POINT('Ctrl Pts',(-0.903192383803698,-0.281092746028013,
1.39907794072174));
#8487=CARTESIAN_POINT('Ctrl Pts',(-0.833097246109156,-1.31780193144713,
0.547568473278941));
#8488=CARTESIAN_POINT('Ctrl Pts',(-0.763002108414612,-1.18981447429149,
-0.787893128290417));
#8489=CARTESIAN_POINT('Ctrl Pts',(-0.692906970720072,-0.0102477773186068,
-1.4269980920415));
#8490=CARTESIAN_POINT('Ctrl Pts',(-0.622811833025528,1.17837584647217,-0.804902064358118));
#8491=CARTESIAN_POINT('Ctrl Pts',(-0.552716695330987,1.3255304759577,0.528590591252869));
#8492=CARTESIAN_POINT('Ctrl Pts',(-0.482621557636444,0.301156902427986,
1.39488664435986));
#8493=CARTESIAN_POINT('Ctrl Pts',(-0.412526419941902,-0.989382806500896,
1.02839305313024));
#8494=CARTESIAN_POINT('Ctrl Pts',(-0.342431282247359,-1.40549163809771,
-0.247080800712783));
#8495=CARTESIAN_POINT('Ctrl Pts',(-0.272336144552818,-0.579396004506808,
-1.30405044948349));
#8496=CARTESIAN_POINT('Ctrl Pts',(-0.202241006858275,0.75876857619037,-1.20872410724841));
#8497=CARTESIAN_POINT('Ctrl Pts',(-0.132145869163733,1.42634198271324,-0.0446361872515408));
#8498=CARTESIAN_POINT('Ctrl Pts',(-0.0620507314691905,0.833246900288591,
1.15800653451465));
#8499=CARTESIAN_POINT('Ctrl Pts',(0.00804440622535185,-0.49620255857664,
1.33890280024981));
#8500=CARTESIAN_POINT('Ctrl Pts',(0.0781395439198939,-1.38729120345278,
0.333033683692492));
#8501=CARTESIAN_POINT('Ctrl Pts',(0.124869635716256,-1.1635642984508,-0.528638978611794));
#8502=CARTESIAN_POINT('Ctrl Pts',(0.148234681614436,-0.89576523912322,-0.820871266629866));
#8503=CARTESIAN_POINT('',(0.,-0.292167722185243,1.17934855836309));
#8504=CARTESIAN_POINT('Ctrl Pts',(-3.05311331771918E-16,-0.293132536858745,
1.18067345457));
#8505=CARTESIAN_POINT('Ctrl Pts',(-2.41399024079808E-16,-0.335932013416244,
1.16561322977037));
#8506=CARTESIAN_POINT('Ctrl Pts',(-3.24049613596376E-16,-0.377726074145918,
1.14807981448758));
#8507=CARTESIAN_POINT('Ctrl Pts',(-1.66533453693773E-16,-0.418289929981307,
1.12802261826284));
#8508=CARTESIAN_POINT('Ctrl Pts',(-4.17758082892349E-18,-0.460100117742301,
1.10734916099787));
#8509=CARTESIAN_POINT('Ctrl Pts',(-2.2251679718906E-16,-0.500603870175662,
1.08399372536458));
#8510=CARTESIAN_POINT('Ctrl Pts',(5.55111512312578E-17,-0.539635460376147,
1.05816525512961));
#8511=CARTESIAN_POINT('Ctrl Pts',(1.43120952673795E-16,-0.551934762971012,
1.05002640735655));
#8512=CARTESIAN_POINT('Ctrl Pts',(-2.97792580155581E-16,-0.564087662460813,
1.04164182529709));
#8513=CARTESIAN_POINT('Ctrl Pts',(-3.05311331771918E-16,-0.576088318506723,
1.03301762701505));
#8514=CARTESIAN_POINT('Ctrl Pts',(-3.10957770648654E-16,-0.585100582018225,
1.02654101880331));
#8515=CARTESIAN_POINT('Ctrl Pts',(-1.87805466987078E-17,-0.594018974805992,
1.01993501166421));
#8516=CARTESIAN_POINT('Ctrl Pts',(0.,-0.602840687031429,1.01320339714505));
#8517=CARTESIAN_POINT('Ctrl Pts',(8.43077134695688E-17,-0.642442217196913,
0.982984520284144));
#8518=CARTESIAN_POINT('Ctrl Pts',(1.70451744334007E-16,-0.680104775291499,
0.950232561947544));
#8519=CARTESIAN_POINT('Ctrl Pts',(2.4980018054066E-16,-0.715630523030677,
0.915211265061402));
#8520=CARTESIAN_POINT('Ctrl Pts',(3.00087345968065E-16,-0.738145007737591,
0.893016476680078));
#8521=CARTESIAN_POINT('Ctrl Pts',(-1.41299001724718E-16,-0.759800462521797,
0.869909521470008));
#8522=CARTESIAN_POINT('Ctrl Pts',(-1.80411241501588E-16,-0.780536780376596,
0.845952761453801));
#8523=CARTESIAN_POINT('Ctrl Pts',(-1.95118881290929E-16,-0.788334398086693,
0.836944139118487));
#8524=CARTESIAN_POINT('Ctrl Pts',(-2.53267376952506E-16,-0.796001963266571,
0.827815325827747));
#8525=CARTESIAN_POINT('Ctrl Pts',(-3.19189119579733E-16,-0.803535968281199,
0.818569564500166));
#8526=CARTESIAN_POINT('Ctrl Pts',(-3.72764038404646E-16,-0.809658890567517,
0.811055489585601));
#8527=CARTESIAN_POINT('Ctrl Pts',(-2.69654453316991E-16,-0.815687771317065,
0.803471295609831));
#8528=CARTESIAN_POINT('Ctrl Pts',(-2.63677968348475E-16,-0.821620162866385,
0.795820485137319));
#8529=CARTESIAN_POINT('Ctrl Pts',(-2.3278733475951E-16,-0.852282890978593,
0.756275772114527));
#8530=CARTESIAN_POINT('Ctrl Pts',(-7.56686568098375E-16,-0.880382544762949,
0.714940607813026));
#8531=CARTESIAN_POINT('Ctrl Pts',(-6.80011602582908E-16,-0.905714588462527,
0.672080427349177));
#8532=CARTESIAN_POINT('Ctrl Pts',(-6.07721418114474E-16,-0.929597978558549,
0.631671275140858));
#8533=CARTESIAN_POINT('Ctrl Pts',(-1.03226703790935E-15,-0.951021292098657,
0.589905394894723));
#8534=CARTESIAN_POINT('Ctrl Pts',(-1.19348975147204E-15,-0.969765382003686,
0.546993657372317));
#8535=CARTESIAN_POINT('Ctrl Pts',(-1.28143536432127E-15,-0.979990122907564,
0.523585671168403));
#8536=CARTESIAN_POINT('Ctrl Pts',(-1.63505974646731E-16,-0.989416779428147,
0.499836614874287));
#8537=CARTESIAN_POINT('Ctrl Pts',(-1.11022302462516E-16,-0.998003181165185,
0.475780845045036));
#8538=CARTESIAN_POINT('Ctrl Pts',(-8.67220820234133E-17,-1.00197873101346,
0.464642895176907));
#8539=CARTESIAN_POINT('Ctrl Pts',(-6.74696253167536E-17,-1.00577408346956,
0.453439201601946));
#8540=CARTESIAN_POINT('Ctrl Pts',(-1.38777878078145E-17,-1.00938468801266,
0.442173233161444));
#8541=CARTESIAN_POINT('Ctrl Pts',(2.2221827891663E-17,-1.01181680160509,
0.434584444456137));
#8542=CARTESIAN_POINT('Ctrl Pts',(4.18926510052434E-16,-1.01416437175746,
0.42696939985124));
#8543=CARTESIAN_POINT('Ctrl Pts',(3.88578058618805E-16,-1.01642375179121,
0.419337791015749));
#8544=CARTESIAN_POINT('Ctrl Pts',(2.15396781121084E-16,-1.02931674310096,
0.37578855851591));
#8545=CARTESIAN_POINT('Ctrl Pts',(-6.59408752454894E-16,-1.03936791753624,
0.331620664795643));
#8546=CARTESIAN_POINT('Ctrl Pts',(-4.85722573273506E-16,-1.04638812315296,
0.287033942557984));
#8547=CARTESIAN_POINT('Ctrl Pts',(-4.42257175970882E-16,-1.04814494702758,
0.275876004686269));
#8548=CARTESIAN_POINT('Ctrl Pts',(4.37223924785986E-16,-1.04971169924956,
0.264691828952297));
#8549=CARTESIAN_POINT('Ctrl Pts',(3.88578058618805E-16,-1.05108489580466,
0.253484558391007));
#8550=CARTESIAN_POINT('Ctrl Pts',(2.4955770282928E-16,-1.05614503746883,
0.212186481653198));
#8551=CARTESIAN_POINT('Ctrl Pts',(1.34271465327458E-16,-1.05857941169269,
0.17057393394923));
#8552=CARTESIAN_POINT('Ctrl Pts',(1.87350135405495E-16,-1.05845449697657,
0.128862808641984));
#8553=CARTESIAN_POINT('Ctrl Pts',(2.13130568122753E-16,-1.05839382561028,
0.108603618689342));
#8554=CARTESIAN_POINT('Ctrl Pts',(3.52349314273582E-16,-1.05772891141692,
0.0883213386068555));
#8555=CARTESIAN_POINT('Ctrl Pts',(3.05311331771918E-16,-1.05646479410987,
0.0680420226442946));
#8556=CARTESIAN_POINT('Ctrl Pts',(2.77282717210464E-16,-1.0557115420596,
0.0559581470090151));
#8557=CARTESIAN_POINT('Ctrl Pts',(2.72979455253999E-16,-1.05474550432587,
0.0438753433176231));
#8558=CARTESIAN_POINT('Ctrl Pts',(2.35922392732846E-16,-1.0535674917508,
0.031799326129942));
#8559=CARTESIAN_POINT('Ctrl Pts',(2.11048989273273E-16,-1.0527767873596,
0.0236936742714747));
#8560=CARTESIAN_POINT('Ctrl Pts',(6.13180887324493E-16,-1.05189085250313,
0.0155945609871946));
#8561=CARTESIAN_POINT('Ctrl Pts',(6.03683769639929E-16,-1.05091130462964,
0.00751183891852238));
#8562=CARTESIAN_POINT('Ctrl Pts',(5.51080620478412E-16,-1.045485731881,
-0.0372571792963943));
#8563=CARTESIAN_POINT('Ctrl Pts',(8.13451426044107E-16,-1.0371851023245,
-0.0816002357585725));
#8564=CARTESIAN_POINT('Ctrl Pts',(7.56339435525888E-16,-1.02611974514107,
-0.125246436326617));
#8565=CARTESIAN_POINT('Ctrl Pts',(6.99580607089161E-16,-1.01512281254834,
-0.16862274290389));
#8566=CARTESIAN_POINT('Ctrl Pts',(-3.72450892574497E-16,-1.0013945728171,
-0.211311849734376));
#8567=CARTESIAN_POINT('Ctrl Pts',(-5.41233724504764E-16,-0.98499986230162,
-0.253021432803562));
#8568=CARTESIAN_POINT('Ctrl Pts',(-6.17890265177582E-16,-0.977553833703354,
-0.27196478334712));
#8569=CARTESIAN_POINT('Ctrl Pts',(-2.71631770704439E-16,-0.969557250286352,
-0.290705625787388));
#8570=CARTESIAN_POINT('Ctrl Pts',(-3.2612801348364E-16,-0.9610137551908,
-0.309213868158789));
#8571=CARTESIAN_POINT('Ctrl Pts',(-3.57229340238859E-16,-0.956137932215719,
-0.319776631099897));
#8572=CARTESIAN_POINT('Ctrl Pts',(-2.54857688098412E-16,-0.951083951554496,
-0.330263600398875));
#8573=CARTESIAN_POINT('Ctrl Pts',(-2.74086309204336E-16,-0.945852299939878,
-0.34066888161227));
#8574=CARTESIAN_POINT('Ctrl Pts',(-2.91171668308026E-16,-0.941203779068372,
-0.349914368593704));
#8575=CARTESIAN_POINT('Ctrl Pts',(-5.05212835795718E-16,-0.93641387616655,
-0.359097063515204));
#8576=CARTESIAN_POINT('Ctrl Pts',(-4.71844785465692E-16,-0.931494000461812,
-0.368193095666921));
#8577=CARTESIAN_POINT('Ctrl Pts',(-3.32738396632977E-16,-0.910983777778045,
-0.406113087180272));
#8578=CARTESIAN_POINT('Ctrl Pts',(2.09944366161902E-16,-0.888179681046059,
-0.442608221198496));
#8579=CARTESIAN_POINT('Ctrl Pts',(8.32667268468867E-17,-0.863152994506025,
-0.477421131302607));
#8580=CARTESIAN_POINT('Ctrl Pts',(-3.89291622173031E-17,-0.839011731465234,
-0.511002389400613));
#8581=CARTESIAN_POINT('Ctrl Pts',(3.08915620636759E-16,-0.81280165934355,
-0.54301893377654));
#8582=CARTESIAN_POINT('Ctrl Pts',(4.23272528138341E-16,-0.784558442664854,
-0.57320193611465));
#8583=CARTESIAN_POINT('Ctrl Pts',(5.22476258772195E-16,-0.760057671169367,
-0.599385456630273));
#8584=CARTESIAN_POINT('Ctrl Pts',(8.10803150113927E-17,-0.734026249237344,
-0.624188862340296));
#8585=CARTESIAN_POINT('Ctrl Pts',(1.38777878078145E-17,-0.706474930361996,
-0.647407317899646));
#8586=CARTESIAN_POINT('Ctrl Pts',(-0.354892650149939,-1.2156153315498,-0.000937869499410686));
#8587=CARTESIAN_POINT('Ctrl Pts',(-0.350738860849079,-1.21620978459426,
-0.0712934765369628));
#8588=CARTESIAN_POINT('Ctrl Pts',(-0.346585071548219,-1.21060532749883,
-0.14155394012693));
#8589=CARTESIAN_POINT('Ctrl Pts',(-0.342431282247359,-1.19845756056642,
-0.210663433200738));
#8590=CARTESIAN_POINT('Ctrl Pts',(-0.319066236349179,-1.13012642690074,
-0.599404016969691));
#8591=CARTESIAN_POINT('Ctrl Pts',(-0.295701190450998,-0.854761215703772,
-0.951727233226591));
#8592=CARTESIAN_POINT('Ctrl Pts',(-0.272336144552818,-0.494051179989093,
-1.11200111764919));
#8593=CARTESIAN_POINT('Ctrl Pts',(-0.248971098654637,-0.133341144274414,
-1.2722750020718));
#8594=CARTESIAN_POINT('Ctrl Pts',(-0.225606052756456,0.312713715957976,
-1.24049955466011));
#8595=CARTESIAN_POINT('Ctrl Pts',(-0.202241006858275,0.64700338049465,-1.03059717762145));
#8596=CARTESIAN_POINT('Ctrl Pts',(-0.178875960960094,0.981293045031325,
-0.82069480058279));
#8597=CARTESIAN_POINT('Ctrl Pts',(-0.155510915061913,1.20381751387228,-0.432665493917164));
#8598=CARTESIAN_POINT('Ctrl Pts',(-0.132145869163732,1.21623056788865,-0.0382103869566515));
#8599=CARTESIAN_POINT('Ctrl Pts',(-0.108780823265552,1.22864362190502,0.356244720003858));
#8600=CARTESIAN_POINT('Ctrl Pts',(-0.0854157773673712,1.03094526109681,
0.757125627259254));
#8601=CARTESIAN_POINT('Ctrl Pts',(-0.0620507314691906,0.710521170881829,
0.987715458509478));
#8602=CARTESIAN_POINT('Ctrl Pts',(-0.0413671543127939,0.426870266808673,
1.19184185256531));
#8603=CARTESIAN_POINT('Ctrl Pts',(-0.0206835771563971,0.0470462558057122,
1.26252090887865));
#8604=CARTESIAN_POINT('Ctrl Pts',(-2.94902990916057E-16,-0.293132536858746,
1.18067345457));
#8605=CARTESIAN_POINT('',(-2.235,-0.557525174626851,-0.780836043637726));
#8606=CARTESIAN_POINT('Ctrl Pts',(-2.235,-0.557525174626855,-0.780836043637723));
#8607=CARTESIAN_POINT('Ctrl Pts',(-2.235,-0.589761389590488,-0.763902150685921));
#8608=CARTESIAN_POINT('Ctrl Pts',(-2.235,-0.620887948635336,-0.745102743152277));
#8609=CARTESIAN_POINT('Ctrl Pts',(-2.235,-0.650719001081195,-0.724483598080833));
#8610=CARTESIAN_POINT('Ctrl Pts',(-2.235,-0.686232768596372,-0.699936575284436));
#8611=CARTESIAN_POINT('Ctrl Pts',(-2.235,-0.719912199030247,-0.672812168345133));
#8612=CARTESIAN_POINT('Ctrl Pts',(-2.235,-0.75168110876748,-0.643417830155717));
#8613=CARTESIAN_POINT('Ctrl Pts',(-2.235,-0.762057019880621,-0.633817467952367));
#8614=CARTESIAN_POINT('Ctrl Pts',(-2.235,-0.772232353877974,-0.623970750017659));
#8615=CARTESIAN_POINT('Ctrl Pts',(-2.235,-0.782182525354984,-0.613909717043614));
#8616=CARTESIAN_POINT('Ctrl Pts',(-2.235,-0.812598374920379,-0.583154984211313));
#8617=CARTESIAN_POINT('Ctrl Pts',(-2.235,-0.840948417922223,-0.550370430406235));
#8618=CARTESIAN_POINT('Ctrl Pts',(-2.235,-0.867164276315998,-0.515863413535596));
#8619=CARTESIAN_POINT('Ctrl Pts',(-2.235,-0.885307489374087,-0.491982137184495));
#8620=CARTESIAN_POINT('Ctrl Pts',(-2.235,-0.90242815802142,-0.467274692073097));
#8621=CARTESIAN_POINT('Ctrl Pts',(-2.235,-0.91849637257373,-0.441830457957078));
#8622=CARTESIAN_POINT('Ctrl Pts',(-2.235,-0.92388138647726,-0.433303215926959));
#8623=CARTESIAN_POINT('Ctrl Pts',(-2.235,-0.929149006146672,-0.424691674581802));
#8624=CARTESIAN_POINT('Ctrl Pts',(-2.235,-0.934295189375141,-0.416003614975756));
#8625=CARTESIAN_POINT('Ctrl Pts',(-2.235,-0.95714587072572,-0.377425882159267));
#8626=CARTESIAN_POINT('Ctrl Pts',(-2.235,-0.977521859790832,-0.337484205077708));
#8627=CARTESIAN_POINT('Ctrl Pts',(-2.235,-0.995355662607526,-0.296493718490565));
#8628=CARTESIAN_POINT('Ctrl Pts',(-2.235,-1.01365427183518,-0.254434887638901));
#8629=CARTESIAN_POINT('Ctrl Pts',(-2.235,-1.02927729005099,-0.211271007625217));
#8630=CARTESIAN_POINT('Ctrl Pts',(-2.235,-1.0421180641197,-0.167300381368861));
#8631=CARTESIAN_POINT('Ctrl Pts',(-2.235,-1.04971059252501,-0.141301307865673));
#8632=CARTESIAN_POINT('Ctrl Pts',(-2.235,-1.05632970833611,-0.115019449284481));
#8633=CARTESIAN_POINT('Ctrl Pts',(-2.235,-1.06194617544159,-0.0885117973462398));
#8634=CARTESIAN_POINT('Ctrl Pts',(-2.235,-1.06506954309429,-0.0737706547279307));
#8635=CARTESIAN_POINT('Ctrl Pts',(-2.235,-1.067882731821,-0.0589596333448952));
#8636=CARTESIAN_POINT('Ctrl Pts',(-2.235,-1.07037988124494,-0.0440882456579739));
#8637=CARTESIAN_POINT('Ctrl Pts',(-2.235,-1.0716748055031,-0.0363765242512822));
#8638=CARTESIAN_POINT('Ctrl Pts',(-2.235,-1.07288442173141,-0.0286499953000482));
#8639=CARTESIAN_POINT('Ctrl Pts',(-2.235,-1.07400675594759,-0.0209196560664691));
#8640=CARTESIAN_POINT('Ctrl Pts',(-2.235,-1.08080241816933,0.0258870558144123));
#8641=CARTESIAN_POINT('Ctrl Pts',(-2.235,-1.08441805875872,0.0729268356242396));
#8642=CARTESIAN_POINT('Ctrl Pts',(-2.235,-1.08475384304639,0.119882946622176));
#8643=CARTESIAN_POINT('Ctrl Pts',(-2.235,-1.08483257546759,0.130892896892274));
#8644=CARTESIAN_POINT('Ctrl Pts',(-2.235,-1.08473080181681,0.141898373671195));
#8645=CARTESIAN_POINT('Ctrl Pts',(-2.235,-1.08444687417653,0.152895498319631));
#8646=CARTESIAN_POINT('Ctrl Pts',(-2.235,-1.08323508593218,0.199830648265685));
#8647=CARTESIAN_POINT('Ctrl Pts',(-2.235,-1.07871004096183,0.246612966455125));
#8648=CARTESIAN_POINT('Ctrl Pts',(-2.235,-1.07107744747181,0.293014825827104));
#8649=CARTESIAN_POINT('Ctrl Pts',(-2.235,-1.06749579235591,0.314789266877131));
#8650=CARTESIAN_POINT('Ctrl Pts',(-2.235,-1.0632289940904,0.336480057213568));
#8651=CARTESIAN_POINT('Ctrl Pts',(-2.235,-1.05829395685729,0.358063870176975));
#8652=CARTESIAN_POINT('Ctrl Pts',(-2.235,-1.05644573327181,0.366147236177911));
#8653=CARTESIAN_POINT('Ctrl Pts',(-2.235,-1.05450349182407,0.374216640931737));
#8654=CARTESIAN_POINT('Ctrl Pts',(-2.235,-1.0524688488774,0.382267600376829));
#8655=CARTESIAN_POINT('Ctrl Pts',(-2.235,-1.04090512293783,0.428024566593539));
#8656=CARTESIAN_POINT('Ctrl Pts',(-2.235,-1.02641643613206,0.472969040823713));
#8657=CARTESIAN_POINT('Ctrl Pts',(-2.235,-1.00923443573082,0.516879291823335));
#8658=CARTESIAN_POINT('Ctrl Pts',(-2.235,-0.991633669262111,0.561859739697787));
#8659=CARTESIAN_POINT('Ctrl Pts',(-2.235,-0.971206522360287,0.605755914128234));
#8660=CARTESIAN_POINT('Ctrl Pts',(-2.235,-0.948146909593293,0.648332705241361));
#8661=CARTESIAN_POINT('Ctrl Pts',(-2.235,-0.935103628555331,0.672415549033863));
#8662=CARTESIAN_POINT('Ctrl Pts',(-2.235,-0.92121713659497,0.696076245707203));
#8663=CARTESIAN_POINT('Ctrl Pts',(-2.235,-0.906515397927934,0.719270808256462));
#8664=CARTESIAN_POINT('Ctrl Pts',(-2.235,-0.895731693398996,0.736283987097004));
#8665=CARTESIAN_POINT('Ctrl Pts',(-2.235,-0.88450926307828,0.753046354789358));
#8666=CARTESIAN_POINT('Ctrl Pts',(-2.235,-0.872857527545231,0.769539831521511));
#8667=CARTESIAN_POINT('Ctrl Pts',(-2.235,-0.867086149421807,0.777709437716325));
#8668=CARTESIAN_POINT('Ctrl Pts',(-2.235,-0.861208513998563,0.785814086476887));
#8669=CARTESIAN_POINT('Ctrl Pts',(-2.235,-0.855236830129837,0.79383707455631));
#8670=CARTESIAN_POINT('Ctrl Pts',(-2.235,-0.825119235334744,0.834300218509289));
#8671=CARTESIAN_POINT('Ctrl Pts',(-2.235,-0.792554804383182,0.872772326773698));
#8672=CARTESIAN_POINT('Ctrl Pts',(-2.235,-0.7577578394247,0.909007312729686));
#8673=CARTESIAN_POINT('Ctrl Pts',(-2.235,-0.723176138298807,0.945018138849895));
#8674=CARTESIAN_POINT('Ctrl Pts',(-2.235,-0.686388893817687,0.978820512031619));
#8675=CARTESIAN_POINT('Ctrl Pts',(-2.235,-0.647559107541456,1.010155505039));
#8676=CARTESIAN_POINT('Ctrl Pts',(-2.235,-0.610523528048654,1.04004260295335));
#8677=CARTESIAN_POINT('Ctrl Pts',(-2.235,-0.571629106455326,1.06768579765986));
#8678=CARTESIAN_POINT('Ctrl Pts',(-2.235,-0.530983509300122,1.09283187766981));
#8679=CARTESIAN_POINT('Ctrl Pts',(-2.235,-0.557525174626851,-0.780836043637726));
#8680=CARTESIAN_POINT('Ctrl Pts',(-2.2143164228436,-0.331791173027909,-0.939557070115845));
#8681=CARTESIAN_POINT('Ctrl Pts',(-2.17026779978903,0.305102622594342,-1.06385016155341));
#8682=CARTESIAN_POINT('Ctrl Pts',(-2.10285413083626,1.05900093864512,-0.381087916994184));
#8683=CARTESIAN_POINT('Ctrl Pts',(-2.03275899314173,0.907151642232085,0.666313302776059));
#8684=CARTESIAN_POINT('Ctrl Pts',(-1.96266385544718,-0.0465745614418721,
1.12446411646007));
#8685=CARTESIAN_POINT('Ctrl Pts',(-1.90278663498807,-0.826057143873035,
0.66703697687178));
#8686=CARTESIAN_POINT('Ctrl Pts',(-1.86627446042713,-0.956397313027637,
0.176203929829702));
#8687=CARTESIAN_POINT('Ctrl Pts',(-1.85312733176438,-0.956897745415108,
-0.000286873987960694));
#8688=CARTESIAN_POINT('Origin',(-2.235,-1.13809670924099E-16,0.));
#8689=CARTESIAN_POINT('',(-2.235,-1.215,-1.48794586096403E-16));
#8690=CARTESIAN_POINT('Origin',(-2.235,0.,0.));
#8691=CARTESIAN_POINT('Origin',(-2.235,0.,0.));
#8692=CARTESIAN_POINT('',(-2.235,0.556433207999849,-0.780144311992978));
#8693=CARTESIAN_POINT('Ctrl Pts',(-2.235,0.532202955181986,1.09392695412892));
#8694=CARTESIAN_POINT('Ctrl Pts',(-2.235,0.570935961351045,1.07029732077084));
#8695=CARTESIAN_POINT('Ctrl Pts',(-2.235,0.608171312273549,1.04445758783552));
#8696=CARTESIAN_POINT('Ctrl Pts',(-2.235,0.643678611685364,1.0164050085206));
#8697=CARTESIAN_POINT('Ctrl Pts',(-2.235,0.680276879397345,0.987490508550553));
#8698=CARTESIAN_POINT('Ctrl Pts',(-2.235,0.715039639510439,0.956224271593212));
#8699=CARTESIAN_POINT('Ctrl Pts',(-2.235,0.747848230138463,0.922845129327136));
#8700=CARTESIAN_POINT('Ctrl Pts',(-2.235,0.758186628312356,0.912326943180031));
#8701=CARTESIAN_POINT('Ctrl Pts',(-2.235,0.768330729852818,0.901598830932486));
#8702=CARTESIAN_POINT('Ctrl Pts',(-2.235,0.778276094069858,0.890667991214823));
#8703=CARTESIAN_POINT('Ctrl Pts',(-2.235,0.785744826798305,0.882459189750435));
#8704=CARTESIAN_POINT('Ctrl Pts',(-2.235,0.793094836869084,0.874143334991178));
#8705=CARTESIAN_POINT('Ctrl Pts',(-2.235,0.800324164370073,0.865724719557378));
#8706=CARTESIAN_POINT('Ctrl Pts',(-2.235,0.832777416305257,0.827932622355924));
#8707=CARTESIAN_POINT('Ctrl Pts',(-2.235,0.862807405761098,0.788065939422894));
#8708=CARTESIAN_POINT('Ctrl Pts',(-2.235,0.890275454946883,0.746423779773389));
#8709=CARTESIAN_POINT('Ctrl Pts',(-2.235,0.907683361818825,0.720033014552966));
#8710=CARTESIAN_POINT('Ctrl Pts',(-2.235,0.924061359764043,0.692928619453533));
#8711=CARTESIAN_POINT('Ctrl Pts',(-2.235,0.939363621583103,0.665184089794141));
#8712=CARTESIAN_POINT('Ctrl Pts',(-2.235,0.945117925016288,0.654750962707512));
#8713=CARTESIAN_POINT('Ctrl Pts',(-2.235,0.95072002395897,0.644227307812222));
#8714=CARTESIAN_POINT('Ctrl Pts',(-2.235,0.956167161564349,0.633617026575594));
#8715=CARTESIAN_POINT('Ctrl Pts',(-2.235,0.960593935695727,0.624994274240761));
#8716=CARTESIAN_POINT('Ctrl Pts',(-2.235,0.964914147803501,0.616322489816617));
#8717=CARTESIAN_POINT('Ctrl Pts',(-2.235,0.969126132571279,0.607605606961102));
#8718=CARTESIAN_POINT('Ctrl Pts',(-2.235,0.990896948251949,0.562549971572965));
#8719=CARTESIAN_POINT('Ctrl Pts',(-2.235,1.00978844472556,0.516275903978842));
#8720=CARTESIAN_POINT('Ctrl Pts',(-2.235,1.02565574506571,0.469085560530428));
#8721=CARTESIAN_POINT('Ctrl Pts',(-2.235,1.04061566397402,0.424593826202019));
#8722=CARTESIAN_POINT('Ctrl Pts',(-2.235,1.05288718297695,0.379286485515974));
#8723=CARTESIAN_POINT('Ctrl Pts',(-2.235,1.06229978775484,0.333415361987417));
#8724=CARTESIAN_POINT('Ctrl Pts',(-2.235,1.06743427542606,0.308393094105121));
#8725=CARTESIAN_POINT('Ctrl Pts',(-2.235,1.07171720862766,0.283203138768487));
#8726=CARTESIAN_POINT('Ctrl Pts',(-2.235,1.07511448199102,0.257887868864709));
#8727=CARTESIAN_POINT('Ctrl Pts',(-2.235,1.07668747296967,0.246166500896409));
#8728=CARTESIAN_POINT('Ctrl Pts',(-2.235,1.07807052747635,0.234418289336243));
#8729=CARTESIAN_POINT('Ctrl Pts',(-2.235,1.07925991542886,0.222647573559399));
#8730=CARTESIAN_POINT('Ctrl Pts',(-2.235,1.08006108948689,0.214718796321534));
#8731=CARTESIAN_POINT('Ctrl Pts',(-2.235,1.08077410511126,0.206781914938808));
#8732=CARTESIAN_POINT('Ctrl Pts',(-2.235,1.08139741040059,0.198847166680972));
#8733=CARTESIAN_POINT('Ctrl Pts',(-2.235,1.08495418750844,0.153568983673532));
#8734=CARTESIAN_POINT('Ctrl Pts',(-2.235,1.08560262210768,0.108276498550504));
#8735=CARTESIAN_POINT('Ctrl Pts',(-2.235,1.08319924414589,0.0632045017416759));
#8736=CARTESIAN_POINT('Ctrl Pts',(-2.235,1.08259781979703,0.0519256281048941));
#8737=CARTESIAN_POINT('Ctrl Pts',(-2.235,1.08180503941071,0.0406606062533197));
#8738=CARTESIAN_POINT('Ctrl Pts',(-2.235,1.08081814896937,0.0294132343569632));
#8739=CARTESIAN_POINT('Ctrl Pts',(-2.235,1.07718136004208,-0.0120344439874117));
#8740=CARTESIAN_POINT('Ctrl Pts',(-2.235,1.07091080750056,-0.0532438047629177));
#8741=CARTESIAN_POINT('Ctrl Pts',(-2.235,1.06211640235717,-0.0940174914631829));
#8742=CARTESIAN_POINT('Ctrl Pts',(-2.235,1.05784493676256,-0.113821377805274));
#8743=CARTESIAN_POINT('Ctrl Pts',(-2.235,1.05297763225743,-0.133522222447208));
#8744=CARTESIAN_POINT('Ctrl Pts',(-2.235,1.04752483525318,-0.153095587959791));
#8745=CARTESIAN_POINT('Ctrl Pts',(-2.235,1.04427566217819,-0.164758822839231));
#8746=CARTESIAN_POINT('Ctrl Pts',(-2.235,1.0408185757323,-0.176376768999421));
#8747=CARTESIAN_POINT('Ctrl Pts',(-2.235,1.03715555713669,-0.187944005245821));
#8748=CARTESIAN_POINT('Ctrl Pts',(-2.235,1.03469686685762,-0.195708162203401));
#8749=CARTESIAN_POINT('Ctrl Pts',(-2.235,1.03214638620948,-0.203446123892296));
#8750=CARTESIAN_POINT('Ctrl Pts',(-2.235,1.02950774573197,-0.211148589345367));
#8751=CARTESIAN_POINT('Ctrl Pts',(-2.235,1.01489274295801,-0.253811299526025));
#8752=CARTESIAN_POINT('Ctrl Pts',(-2.235,0.997554076096989,-0.295459604389543));
#8753=CARTESIAN_POINT('Ctrl Pts',(-2.235,0.977655983421763,-0.335851464592034));
#8754=CARTESIAN_POINT('Ctrl Pts',(-2.235,0.957880950340033,-0.375993521661219));
#8755=CARTESIAN_POINT('Ctrl Pts',(-2.235,0.935577178122234,-0.414895529727038));
#8756=CARTESIAN_POINT('Ctrl Pts',(-2.235,0.910868861591031,-0.452285030065642));
#8757=CARTESIAN_POINT('Ctrl Pts',(-2.235,0.899647016373272,-0.469266323997152));
#8758=CARTESIAN_POINT('Ctrl Pts',(-2.235,0.887928751362612,-0.485935068401997));
#8759=CARTESIAN_POINT('Ctrl Pts',(-2.235,0.875723886356509,-0.502262586036078));
#8760=CARTESIAN_POINT('Ctrl Pts',(-2.235,0.868758508523048,-0.511580782455866));
#8761=CARTESIAN_POINT('Ctrl Pts',(-2.235,0.861634625064288,-0.520787800698161));
#8762=CARTESIAN_POINT('Ctrl Pts',(-2.235,0.854353937554375,-0.529877976291384));
#8763=CARTESIAN_POINT('Ctrl Pts',(-2.235,0.847884766054935,-0.537954947702741));
#8764=CARTESIAN_POINT('Ctrl Pts',(-2.235,0.841290357473231,-0.545941104261957));
#8765=CARTESIAN_POINT('Ctrl Pts',(-2.235,0.8345868346318,-0.55381546899887));
#8766=CARTESIAN_POINT('Ctrl Pts',(-2.235,0.806640848200088,-0.586642520580773));
#8767=CARTESIAN_POINT('Ctrl Pts',(-2.235,0.776747360164672,-0.617598927517484));
#8768=CARTESIAN_POINT('Ctrl Pts',(-2.235,0.745029604371381,-0.646447765737017));
#8769=CARTESIAN_POINT('Ctrl Pts',(-2.235,0.71443401474895,-0.674275939363204));
#8770=CARTESIAN_POINT('Ctrl Pts',(-2.235,0.682140147959964,-0.700143461935094));
#8771=CARTESIAN_POINT('Ctrl Pts',(-2.235,0.648238779596853,-0.723794792910752));
#8772=CARTESIAN_POINT('Ctrl Pts',(-2.235,0.618829490798728,-0.744312219100546));
#8773=CARTESIAN_POINT('Ctrl Pts',(-2.235,0.588209931826527,-0.7631614344557));
#8774=CARTESIAN_POINT('Ctrl Pts',(-2.235,0.556433207999848,-0.780144311992979));
#8775=CARTESIAN_POINT('Origin',(-2.235,0.,0.));
#8776=CARTESIAN_POINT('Origin',(-3.06687266823562,0.,0.));
#8777=CARTESIAN_POINT('Ctrl Pts',(-2.235,0.556433207999848,-0.780144311992979));
#8778=CARTESIAN_POINT('Ctrl Pts',(-2.21163495410182,0.81094560401685,-0.598614886200353));
#8779=CARTESIAN_POINT('Ctrl Pts',(-2.16490486230546,1.12483260886138,0.029436645387845));
#8780=CARTESIAN_POINT('Ctrl Pts',(-2.09480972461091,0.602343789565177,0.951528243211824));
#8781=CARTESIAN_POINT('Ctrl Pts',(-2.02471458691638,-0.45292157341433,1.02997591440566));
#8782=CARTESIAN_POINT('Ctrl Pts',(-1.97373556812461,-0.929108146284966,
0.425949523674369));
#8783=CARTESIAN_POINT('Ctrl Pts',(-1.94612159523103,-0.959171617511514,
0.0575656004424785));
#8784=CARTESIAN_POINT('Ctrl Pts',(-1.94187266823562,-0.958689328197825,
0.000800959330899747));
#8785=CARTESIAN_POINT('Ctrl Pts',(-2.38323468161444,0.70552188648037,-0.989173325407221));
#8786=CARTESIAN_POINT('Ctrl Pts',(-2.35986963571626,1.02822740295379,-0.759005569249601));
#8787=CARTESIAN_POINT('Ctrl Pts',(-2.31313954391989,1.42621614376893,0.0373237924823694));
#8788=CARTESIAN_POINT('Ctrl Pts',(-2.24304440622535,0.763733581342751,1.20647724028423));
#8789=CARTESIAN_POINT('Ctrl Pts',(-2.17294926853081,-0.574275723139484,
1.30594389355896));
#8790=CARTESIAN_POINT('Ctrl Pts',(-2.10285413083627,-1.404453333381,0.252891972003963));
#8791=CARTESIAN_POINT('Ctrl Pts',(-2.03275899314172,-0.99349569060003,-1.02455353802336));
#8792=CARTESIAN_POINT('Ctrl Pts',(-1.96266385544718,0.295607537464514,-1.39601730052373));
#8793=CARTESIAN_POINT('Ctrl Pts',(-1.89256871775264,1.3234073776496,-0.533899580371048));
#8794=CARTESIAN_POINT('Ctrl Pts',(-1.8224735800581,1.18157746100638,0.800215952773212));
#8795=CARTESIAN_POINT('Ctrl Pts',(-1.75237844236356,-0.00456266479474856,
1.42701921510532));
#8796=CARTESIAN_POINT('Ctrl Pts',(-1.68228330466901,-1.18666438626039,0.792632946367487));
#8797=CARTESIAN_POINT('Ctrl Pts',(-1.61218816697447,-1.31997416439636,-0.542314941584932));
#8798=CARTESIAN_POINT('Ctrl Pts',(-1.54209302927993,-0.286665770377846,
-1.39794551284947));
#8799=CARTESIAN_POINT('Ctrl Pts',(-1.47199789158539,1.00000206223092,-1.01805219163445));
#8800=CARTESIAN_POINT('Ctrl Pts',(-1.40190275389085,1.40285079895742,0.261616380034874));
#8801=CARTESIAN_POINT('Ctrl Pts',(-1.3318076161963,0.565834901448313,1.31006237061056));
#8802=CARTESIAN_POINT('Ctrl Pts',(-1.26171247850176,-0.771275778959115,
1.20065271063163));
#8803=CARTESIAN_POINT('Ctrl Pts',(-1.19161734080722,-1.4267193361598,0.0300846251506579));
#8804=CARTESIAN_POINT('Ctrl Pts',(-1.12152220311268,-0.821203001667309,
-1.1670727864228));
#8805=CARTESIAN_POINT('Ctrl Pts',(-1.05142706541813,0.510107032224125,-1.33275030154274));
#8806=CARTESIAN_POINT('Ctrl Pts',(-0.981331927723592,1.39057553246452,-0.320520175572548));
#8807=CARTESIAN_POINT('Ctrl Pts',(-0.911236790029049,1.04202855526106,0.974992758628685));
#8808=CARTESIAN_POINT('Ctrl Pts',(-0.841141652334507,-0.22748139059697,
1.40878711583204));
#8809=CARTESIAN_POINT('Ctrl Pts',(-0.771046514639965,-1.29593988473495,
0.597475610961073));
#8810=CARTESIAN_POINT('Ctrl Pts',(-0.700951376945422,-1.21902254189685,
-0.741905247072227));
#8811=CARTESIAN_POINT('Ctrl Pts',(-0.63085623925088,-0.0647137586129758,
-1.42555841256541));
#8812=CARTESIAN_POINT('Ctrl Pts',(-0.560761101556339,1.14679453675556,-0.84931334494321));
#8813=CARTESIAN_POINT('Ctrl Pts',(-0.490665963861794,1.34473723177141,0.477637547336413));
#8814=CARTESIAN_POINT('Ctrl Pts',(-0.420570826167255,0.354193056453061,
1.38231523117118));
#8815=CARTESIAN_POINT('Ctrl Pts',(-0.35047568847271,-0.949423132758245,
1.06552304268868));
#8816=CARTESIAN_POINT('Ctrl Pts',(-0.280380550778169,-1.4138654371531,-0.193463280166926));
#8817=CARTESIAN_POINT('Ctrl Pts',(-0.210285413083626,-0.628816545074822,
-1.28057479748412));
#8818=CARTESIAN_POINT('Ctrl Pts',(-0.140190275389084,0.71219637134211,-1.23759954882087));
#8819=CARTESIAN_POINT('Ctrl Pts',(-0.0700951376945416,1.42337502914537,
-0.097411912196576));
#8820=CARTESIAN_POINT('Ctrl Pts',(-0.0233650458981805,1.05930884981436,
0.714986578225072));
#8821=CARTESIAN_POINT('Ctrl Pts',(0.,0.746592769117024,0.958553199933198));
#8822=CARTESIAN_POINT('Ctrl Pts',(-2.33382312107629,0.655825660320196,-0.919496987602474));
#8823=CARTESIAN_POINT('Ctrl Pts',(-2.31045807517811,0.955800136641479,-0.705542008233185));
#8824=CARTESIAN_POINT('Ctrl Pts',(-2.26372798338175,1.32575496546642,0.0346947434508616));
#8825=CARTESIAN_POINT('Ctrl Pts',(-2.19363284568721,0.709936984083557,1.1214942412601));
#8826=CARTESIAN_POINT('Ctrl Pts',(-2.12353770799267,-0.533824339897765,
1.21395456717453));
#8827=CARTESIAN_POINT('Ctrl Pts',(-2.05344257029812,-1.30552510475396,0.235078525141954));
#8828=CARTESIAN_POINT('Ctrl Pts',(-1.98334743260358,-0.923514889897269,
-0.952385054926656));
#8829=CARTESIAN_POINT('Ctrl Pts',(-1.91325229490904,0.274785250703467,-1.29768329725639));
#8830=CARTESIAN_POINT('Ctrl Pts',(-1.8431571572145,1.23018794165192,-0.49629225053284));
#8831=CARTESIAN_POINT('Ctrl Pts',(-1.77306201951995,1.09834837647596,0.743849575304207));
#8832=CARTESIAN_POINT('Ctrl Pts',(-1.70296688182541,-0.00424127544329419,
1.32650146929509));
#8833=CARTESIAN_POINT('Ctrl Pts',(-1.63287174413087,-1.10307698401832,0.736800707964236));
#8834=CARTESIAN_POINT('Ctrl Pts',(-1.56277660643633,-1.22699656036104,-0.504114842476036));
#8835=CARTESIAN_POINT('Ctrl Pts',(-1.49268146874178,-0.266473332368378,
-1.29947568831611));
#8836=CARTESIAN_POINT('Ctrl Pts',(-1.42258633104725,0.929562959493534,-0.946341656599571));
#8837=CARTESIAN_POINT('Ctrl Pts',(-1.3524911933527,1.3040354511845,0.243188394966574));
#8838=CARTESIAN_POINT('Ctrl Pts',(-1.28239605565816,0.525978080886761,1.21778294299622));
#8839=CARTESIAN_POINT('Ctrl Pts',(-1.21230091796361,-0.716947917162748,
1.11607998540401));
#8840=CARTESIAN_POINT('Ctrl Pts',(-1.14220578026907,-1.32622271350986,0.027965495518989));
#8841=CARTESIAN_POINT('Ctrl Pts',(-1.07211064257453,-0.763358318353705,
-1.08486539604858));
#8842=CARTESIAN_POINT('Ctrl Pts',(-1.00201550487999,0.474175624673083,-1.23887275972625));
#8843=CARTESIAN_POINT('Ctrl Pts',(-0.931920367185447,1.29262484166609,-0.297943068555193));
#8844=CARTESIAN_POINT('Ctrl Pts',(-0.861825229490902,0.96862915016825,0.906315285164235));
#8845=CARTESIAN_POINT('Ctrl Pts',(-0.791730091796362,-0.211457838598131,
1.30955362008722));
#8846=CARTESIAN_POINT('Ctrl Pts',(-0.721634954101819,-1.20465523030266,
0.555390051807641));
#8847=CARTESIAN_POINT('Ctrl Pts',(-0.651539816407277,-1.1331558649059,-0.689646214922488));
#8848=CARTESIAN_POINT('Ctrl Pts',(-0.581444678712735,-0.0601553889219246,
-1.32514356416317));
#8849=CARTESIAN_POINT('Ctrl Pts',(-0.511349541018193,1.06601552514733,-0.789488598354958));
#8850=CARTESIAN_POINT('Ctrl Pts',(-0.44125440332365,1.25001534308628,0.443993256450644));
#8851=CARTESIAN_POINT('Ctrl Pts',(-0.371159265629109,0.329244066811271,
1.28494638738429));
#8852=CARTESIAN_POINT('Ctrl Pts',(-0.301064127934565,-0.882546757083162,
0.990468710395036));
#8853=CARTESIAN_POINT('Ctrl Pts',(-0.230968990240023,-1.31427422974869,
-0.179835928402081));
#8854=CARTESIAN_POINT('Ctrl Pts',(-0.160873852545481,-0.584523363196095,
-1.1903724437793));
#8855=CARTESIAN_POINT('Ctrl Pts',(-0.0907787148509382,0.662030001426586,
-1.15042432682916));
#8856=CARTESIAN_POINT('Ctrl Pts',(-0.0206835771563963,1.32311397599501,
-0.0905503186557062));
#8857=CARTESIAN_POINT('Ctrl Pts',(0.026046514639965,0.984692238788337,0.664623669045569));
#8858=CARTESIAN_POINT('Ctrl Pts',(0.0494115605381455,0.694003552801305,
0.891033711844625));
#8859=CARTESIAN_POINT('Ctrl Pts',(-2.28441156053815,0.606129434160022,-0.849820649797726));
#8860=CARTESIAN_POINT('Ctrl Pts',(-2.26104651463996,0.883372870329165,-0.652078447216769));
#8861=CARTESIAN_POINT('Ctrl Pts',(-2.2143164228436,1.2252937871639,0.0320656944193542));
#8862=CARTESIAN_POINT('Ctrl Pts',(-2.14422128514906,0.656140386824367,1.03651124223596));
#8863=CARTESIAN_POINT('Ctrl Pts',(-2.07412614745452,-0.493372956656047,
1.1219652407901));
#8864=CARTESIAN_POINT('Ctrl Pts',(-2.00403100975998,-1.20659687612692,0.217265078279945));
#8865=CARTESIAN_POINT('Ctrl Pts',(-1.93393587206544,-0.85353408919451,-0.880216571829947));
#8866=CARTESIAN_POINT('Ctrl Pts',(-1.86384073437089,0.253962963942421,-1.19934929398904));
#8867=CARTESIAN_POINT('Ctrl Pts',(-1.79374559667635,1.13696850565425,-0.458684920694631));
#8868=CARTESIAN_POINT('Ctrl Pts',(-1.72365045898181,1.01511929194553,0.687483197835202));
#8869=CARTESIAN_POINT('Ctrl Pts',(-1.65355532128727,-0.00391988609183947,
1.22598372348486));
#8870=CARTESIAN_POINT('Ctrl Pts',(-1.58346018359272,-1.01948958177625,0.680968469560984));
#8871=CARTESIAN_POINT('Ctrl Pts',(-1.51336504589818,-1.13401895632571,-0.465914743367139));
#8872=CARTESIAN_POINT('Ctrl Pts',(-1.44326990820364,-0.246280894358909,
-1.20100586378275));
#8873=CARTESIAN_POINT('Ctrl Pts',(-1.37317477050909,0.859123856756142,-0.874631121564689));
#8874=CARTESIAN_POINT('Ctrl Pts',(-1.30307963281455,1.20522010341157,0.224760409898275));
#8875=CARTESIAN_POINT('Ctrl Pts',(-1.23298449512001,0.48612126032521,1.12550351538188));
#8876=CARTESIAN_POINT('Ctrl Pts',(-1.16288935742547,-0.662620055366384,
1.0315072601764));
#8877=CARTESIAN_POINT('Ctrl Pts',(-1.09279421973093,-1.22572609085992,0.0258463658873193));
#8878=CARTESIAN_POINT('Ctrl Pts',(-1.02269908203638,-0.705513635040103,
-1.00265800567435));
#8879=CARTESIAN_POINT('Ctrl Pts',(-0.952603944341843,0.438244217122043,
-1.14499521790977));
#8880=CARTESIAN_POINT('Ctrl Pts',(-0.8825088066473,1.19467415086766,-0.275365961537841));
#8881=CARTESIAN_POINT('Ctrl Pts',(-0.812413668952758,0.895229745075445,
0.837637811699788));
#8882=CARTESIAN_POINT('Ctrl Pts',(-0.742318531258216,-0.195434286599291,
1.2103201243424));
#8883=CARTESIAN_POINT('Ctrl Pts',(-0.672223393563674,-1.11337057587037,
0.51330449265421));
#8884=CARTESIAN_POINT('Ctrl Pts',(-0.602128255869132,-1.04728918791495,
-0.637387182772751));
#8885=CARTESIAN_POINT('Ctrl Pts',(-0.53203311817459,-0.0555970192308733,
-1.22472871576093));
#8886=CARTESIAN_POINT('Ctrl Pts',(-0.461937980480047,0.985236513539103,
-0.72966385176671));
#8887=CARTESIAN_POINT('Ctrl Pts',(-0.391842842785505,1.15529345440114,0.410348965564877));
#8888=CARTESIAN_POINT('Ctrl Pts',(-0.321747705090963,0.304295077169481,
1.18757754359741));
#8889=CARTESIAN_POINT('Ctrl Pts',(-0.25165256739642,-0.815670381408078,
0.915414378101397));
#8890=CARTESIAN_POINT('Ctrl Pts',(-0.181557429701878,-1.21468302234429,
-0.166208576637237));
#8891=CARTESIAN_POINT('Ctrl Pts',(-0.111462292007335,-0.540230181317368,
-1.10017009007449));
#8892=CARTESIAN_POINT('Ctrl Pts',(-0.0413671543127928,0.611863631511061,
-1.06324910483746));
#8893=CARTESIAN_POINT('Ctrl Pts',(0.0287279833817493,1.22285292284465,-0.0836887251148355));
#8894=CARTESIAN_POINT('Ctrl Pts',(0.0754580751781104,0.910075627762319,
0.614260759866067));
#8895=CARTESIAN_POINT('Ctrl Pts',(0.0988231210762909,0.641414336485586,
0.823514223756052));
#8896=CARTESIAN_POINT('Ctrl Pts',(-2.235,0.556433207999848,-0.780144311992979));
#8897=CARTESIAN_POINT('Ctrl Pts',(-2.21163495410182,0.81094560401685,-0.598614886200353));
#8898=CARTESIAN_POINT('Ctrl Pts',(-2.16490486230546,1.12483260886138,0.029436645387845));
#8899=CARTESIAN_POINT('Ctrl Pts',(-2.09480972461091,0.602343789565177,0.951528243211824));
#8900=CARTESIAN_POINT('Ctrl Pts',(-2.02471458691638,-0.45292157341433,1.02997591440566));
#8901=CARTESIAN_POINT('Ctrl Pts',(-1.95461944922183,-1.10766864749988,0.199451631417939));
#8902=CARTESIAN_POINT('Ctrl Pts',(-1.88452431152729,-0.78355328849175,-0.808048088733242));
#8903=CARTESIAN_POINT('Ctrl Pts',(-1.81442917383274,0.233140677181374,-1.1010152907217));
#8904=CARTESIAN_POINT('Ctrl Pts',(-1.74433403613821,1.04374906965657,-0.421077590856424));
#8905=CARTESIAN_POINT('Ctrl Pts',(-1.67423889844366,0.931890207415111,0.631116820366198));
#8906=CARTESIAN_POINT('Ctrl Pts',(-1.60414376074912,-0.00359849674038535,
1.12546597767462));
#8907=CARTESIAN_POINT('Ctrl Pts',(-1.53404862305458,-0.935902179534174,
0.625136231157733));
#8908=CARTESIAN_POINT('Ctrl Pts',(-1.46395348536004,-1.04104135229038,-0.427714644258242));
#8909=CARTESIAN_POINT('Ctrl Pts',(-1.39385834766549,-0.226088456349441,
-1.10253603924939));
#8910=CARTESIAN_POINT('Ctrl Pts',(-1.32376320997095,0.788684754018751,-0.802920586529807));
#8911=CARTESIAN_POINT('Ctrl Pts',(-1.25366807227641,1.10640475563864,0.206332424829975));
#8912=CARTESIAN_POINT('Ctrl Pts',(-1.18357293458187,0.446264439763658,1.03322408776754));
#8913=CARTESIAN_POINT('Ctrl Pts',(-1.11347779688732,-0.608292193570018,
0.946934534948777));
#8914=CARTESIAN_POINT('Ctrl Pts',(-1.04338265919278,-1.12522946820998,0.0237272362556514));
#8915=CARTESIAN_POINT('Ctrl Pts',(-0.973287521498239,-0.6476689517265,-0.920450615300125));
#8916=CARTESIAN_POINT('Ctrl Pts',(-0.903192383803697,0.402312809571003,
-1.05111767609328));
#8917=CARTESIAN_POINT('Ctrl Pts',(-0.833097246109155,1.09672346006924,-0.252788854520488));
#8918=CARTESIAN_POINT('Ctrl Pts',(-0.763002108414613,0.821830339982639,
0.76896033823534));
#8919=CARTESIAN_POINT('Ctrl Pts',(-0.69290697072007,-0.17941073460045,1.11108662859757));
#8920=CARTESIAN_POINT('Ctrl Pts',(-0.622811833025529,-1.02208592143808,
0.47121893350078));
#8921=CARTESIAN_POINT('Ctrl Pts',(-0.552716695330986,-0.961422510923996,
-0.585128150623014));
#8922=CARTESIAN_POINT('Ctrl Pts',(-0.482621557636444,-0.0510386495398221,
-1.12431386735868));
#8923=CARTESIAN_POINT('Ctrl Pts',(-0.412526419941902,0.904457501930876,
-0.669839105178461));
#8924=CARTESIAN_POINT('Ctrl Pts',(-0.342431282247359,1.06057156571601,0.37670467467911));
#8925=CARTESIAN_POINT('Ctrl Pts',(-0.272336144552818,0.279346087527691,
1.09020869981052));
#8926=CARTESIAN_POINT('Ctrl Pts',(-0.202241006858274,-0.748794005732996,
0.840360045807757));
#8927=CARTESIAN_POINT('Ctrl Pts',(-0.132145869163732,-1.11509181493988,
-0.152581224872393));
#8928=CARTESIAN_POINT('Ctrl Pts',(-0.0620507314691897,-0.49593699943864,
-1.00996773636968));
#8929=CARTESIAN_POINT('Ctrl Pts',(0.00804440622535258,0.561697261595537,
-0.976073882845758));
#8930=CARTESIAN_POINT('Ctrl Pts',(0.0781395439198948,1.12259186969428,-0.0768271315739657));
#8931=CARTESIAN_POINT('Ctrl Pts',(0.124869635716256,0.835459016736301,0.563897850686564));
#8932=CARTESIAN_POINT('Ctrl Pts',(0.148234681614436,0.588825120169867,0.755994735667479));
#8933=CARTESIAN_POINT('',(0.,0.746592769117024,0.958553199933198));
#8934=CARTESIAN_POINT('Ctrl Pts',(0.,0.382997178453079,-0.879688698994096));
#8935=CARTESIAN_POINT('Ctrl Pts',(-9.804104464095E-17,0.4180497090205,-0.869827137061451));
#8936=CARTESIAN_POINT('Ctrl Pts',(2.83567237026956E-16,0.452404690302672,
-0.85791012243036));
#8937=CARTESIAN_POINT('Ctrl Pts',(8.60422844084496E-16,0.485870814430818,
-0.843943792735025));
#8938=CARTESIAN_POINT('Ctrl Pts',(1.54716742777456E-15,0.525712118217974,
-0.827316926054773));
#8939=CARTESIAN_POINT('Ctrl Pts',(2.72305014732216E-15,0.56429503081299,
-0.807787628815318));
#8940=CARTESIAN_POINT('Ctrl Pts',(3.27515792264421E-15,0.601481112419859,
-0.785640792695669));
#8941=CARTESIAN_POINT('Ctrl Pts',(3.45547965866087E-15,0.613626311402242,
-0.77840750217727));
#8942=CARTESIAN_POINT('Ctrl Pts',(1.97546578491965E-15,0.625626535869127,
-0.770891537608958));
#8943=CARTESIAN_POINT('Ctrl Pts',(1.99840144432528E-15,0.637451076083524,
-0.76311912782532));
#8944=CARTESIAN_POINT('Ctrl Pts',(2.068511555245E-15,0.673596530257937,
-0.73936029436834));
#8945=CARTESIAN_POINT('Ctrl Pts',(2.62962033288778E-15,0.708143337648631,
-0.713186494829503));
#8946=CARTESIAN_POINT('Ctrl Pts',(2.58126853225349E-15,0.740960712846234,
-0.684884151557313));
#8947=CARTESIAN_POINT('Ctrl Pts',(2.54780568648073E-15,0.763672643953208,
-0.665296940005706));
#8948=CARTESIAN_POINT('Ctrl Pts',(2.36504271574013E-15,0.785556143128117,
-0.644689014679008));
#8949=CARTESIAN_POINT('Ctrl Pts',(2.16493489801906E-15,0.806563371679136,
-0.623141582851505));
#8950=CARTESIAN_POINT('Ctrl Pts',(2.09787202592262E-15,0.813603601778398,
-0.615920312432832));
#8951=CARTESIAN_POINT('Ctrl Pts',(2.43023859382518E-15,0.820546530101037,
-0.608592177634928));
#8952=CARTESIAN_POINT('Ctrl Pts',(2.45636844198316E-15,0.827386584885893,
-0.601163949164734));
#8953=CARTESIAN_POINT('Ctrl Pts',(2.57239349865007E-15,0.857758661264587,
-0.568180189596812));
#8954=CARTESIAN_POINT('Ctrl Pts',(2.64260608659013E-15,0.885993699958357,
-0.533347772836182));
#8955=CARTESIAN_POINT('Ctrl Pts',(2.45636844198316E-15,0.91196016345517,
-0.496960911841512));
#8956=CARTESIAN_POINT('Ctrl Pts',(2.26527696128891E-15,0.938603380343306,
-0.459625714867984));
#8957=CARTESIAN_POINT('Ctrl Pts',(2.23712577659718E-15,0.96285922821364,
-0.420653328397313));
#8958=CARTESIAN_POINT('Ctrl Pts',(2.27595720048157E-15,0.98456136594598,
-0.3803133590392));
#8959=CARTESIAN_POINT('Ctrl Pts',(2.29891753903009E-15,0.997393458610018,
-0.356461044062117));
#8960=CARTESIAN_POINT('Ctrl Pts',(2.5501319721175E-15,1.00933220658872,
-0.332129738518424));
#8961=CARTESIAN_POINT('Ctrl Pts',(2.5951463200613E-15,1.02033716389955,
-0.307369109439727));
#8962=CARTESIAN_POINT('Ctrl Pts',(2.62017925710253E-15,1.026457132667,-0.293599471598876));
#8963=CARTESIAN_POINT('Ctrl Pts',(2.04833619180827E-15,1.03228822883295,
-0.279696991010135));
#8964=CARTESIAN_POINT('Ctrl Pts',(2.09554595897998E-15,1.03782274236849,
-0.26566975374606));
#8965=CARTESIAN_POINT('Ctrl Pts',(2.12002711331586E-15,1.04069272644498,
-0.258395772514194));
#8966=CARTESIAN_POINT('Ctrl Pts',(1.99819100377786E-15,1.04348234508209,
-0.251089570609367));
#8967=CARTESIAN_POINT('Ctrl Pts',(2.02615701994091E-15,1.04618738106416,
-0.243761494361897));
#8968=CARTESIAN_POINT('Ctrl Pts',(2.19548911505624E-15,1.06256616764341,
-0.19939055153921));
#8969=CARTESIAN_POINT('Ctrl Pts',(1.98314379665189E-15,1.0758828874101,
-0.15413046122802));
#8970=CARTESIAN_POINT('Ctrl Pts',(1.95676808090184E-15,1.08597403613616,
-0.108270278580235));
#8971=CARTESIAN_POINT('Ctrl Pts',(1.95058373071767E-15,1.08834012159423,
-0.0975173787654368));
#8972=CARTESIAN_POINT('Ctrl Pts',(2.10123556114942E-15,1.09052871862687,
-0.0867313252073607));
#8973=CARTESIAN_POINT('Ctrl Pts',(2.09554595897998E-15,1.09253740899759,
-0.0759155690421767));
#8974=CARTESIAN_POINT('Ctrl Pts',(2.07179073811209E-15,1.10111046158471,
-0.0297541258821798));
#8975=CARTESIAN_POINT('Ctrl Pts',(1.30472882156592E-15,1.10641089348326,
0.0169467036787));
#8976=CARTESIAN_POINT('Ctrl Pts',(1.22818422099158E-15,1.10859258913964,
0.063921494218668));
#8977=CARTESIAN_POINT('Ctrl Pts',(1.19226506616542E-15,1.10961636695646,
0.0859647835123772));
#8978=CARTESIAN_POINT('Ctrl Pts',(2.11933526040146E-15,1.10995258343241,
0.108068701556671));
#8979=CARTESIAN_POINT('Ctrl Pts',(2.1163626406917E-15,1.10961292324264,
0.130206916536899));
#8980=CARTESIAN_POINT('Ctrl Pts',(2.11524936280964E-15,1.10948571686793,
0.138497914879223));
#8981=CARTESIAN_POINT('Ctrl Pts',(1.62000664896157E-15,1.10926364458773,
0.14679480473991));
#8982=CARTESIAN_POINT('Ctrl Pts',(1.65145674912992E-15,1.10894735514218,
0.155092863980238));
#8983=CARTESIAN_POINT('Ctrl Pts',(1.83020083750486E-15,1.10714974978308,
0.202254209294043));
#8984=CARTESIAN_POINT('Ctrl Pts',(2.16858310538254E-15,1.10232217765626,
0.249228958863479));
#8985=CARTESIAN_POINT('Ctrl Pts',(2.07472927726826E-15,1.09464512145237,
0.295752061004661));
#8986=CARTESIAN_POINT('Ctrl Pts',(1.97858800625884E-15,1.08678095697574,
0.343409042728499));
#8987=CARTESIAN_POINT('Ctrl Pts',(1.28761435872327E-15,1.07592674328964,
0.390593086867689));
#8988=CARTESIAN_POINT('Ctrl Pts',(1.49880108324396E-15,1.06222327329097,
0.437033900468828));
#8989=CARTESIAN_POINT('Ctrl Pts',(1.61825517673179E-15,1.05447214409454,
0.463302338042979));
#8990=CARTESIAN_POINT('Ctrl Pts',(1.02429453254145E-15,1.0458084623023,
0.489333167506977));
#8991=CARTESIAN_POINT('Ctrl Pts',(1.02001740387436E-15,1.0362504352041,
0.515077548476332));
#8992=CARTESIAN_POINT('Ctrl Pts',(1.01688012972392E-15,1.02923962171721,
0.533961053561356));
#8993=CARTESIAN_POINT('Ctrl Pts',(2.54700031510392E-17,1.02174752170026,
0.552690444009813));
#8994=CARTESIAN_POINT('Ctrl Pts',(-3.12250225675825E-17,1.013779590733,
0.571246076127072));
#8995=CARTESIAN_POINT('Ctrl Pts',(-5.93072175778668E-17,1.00983291307628,
0.58043705669461));
#8996=CARTESIAN_POINT('Ctrl Pts',(1.75936158409219E-15,1.00576879585552,
0.589586591730184));
#8997=CARTESIAN_POINT('Ctrl Pts',(1.72084568816899E-15,1.00159570819879,
0.598675804818873));
#8998=CARTESIAN_POINT('Ctrl Pts',(1.52659355619868E-15,0.980549042795107,
0.644516592838733));
#8999=CARTESIAN_POINT('Ctrl Pts',(4.67366350146491E-16,0.956695047628213,
0.688918576168094));
#9000=CARTESIAN_POINT('Ctrl Pts',(4.71844785465692E-16,0.930192175349853,
0.731596486069531));
#9001=CARTESIAN_POINT('Ctrl Pts',(4.76295512086431E-16,0.903853280006282,
0.774010341842218));
#9002=CARTESIAN_POINT('Ctrl Pts',(7.39197774204125E-16,0.874897873665825,
0.814722558425196));
#9003=CARTESIAN_POINT('Ctrl Pts',(8.03176969377262E-16,0.843431559477603,
0.853445973895038));
#9004=CARTESIAN_POINT('Ctrl Pts',(8.64199954607425E-16,0.813419171532439,
0.890380142946133));
#9005=CARTESIAN_POINT('Ctrl Pts',(5.51860040342344E-17,0.781122019338172,
0.925505907275885));
#9006=CARTESIAN_POINT('Ctrl Pts',(0.,0.746592769117024,0.958553199933198));
#9007=CARTESIAN_POINT('Ctrl Pts',(0.,0.746592769117024,0.958553199933198));
#9008=CARTESIAN_POINT('Ctrl Pts',(-0.0233650458981805,1.05930884981436,
0.714986578225072));
#9009=CARTESIAN_POINT('Ctrl Pts',(-0.0467300917963609,1.24134193947986,
0.308787333014251));
#9010=CARTESIAN_POINT('Ctrl Pts',(-0.0700951376945414,1.21382870801208,
-0.0843435623618732));
#9011=CARTESIAN_POINT('Ctrl Pts',(-0.0934601835927222,1.18631547654429,
-0.477474457738003));
#9012=CARTESIAN_POINT('Ctrl Pts',(-0.116825229490903,0.949255923943199,
-0.857537003279436));
#9013=CARTESIAN_POINT('Ctrl Pts',(-0.140190275389084,0.607223994906499,
-1.05473081749403));
#9014=CARTESIAN_POINT('Ctrl Pts',(-0.163555321287265,0.265192065869799,
-1.25192463170862));
#9015=CARTESIAN_POINT('Ctrl Pts',(-0.186920367185445,-0.181812239602512,
-1.26624971459637));
#9016=CARTESIAN_POINT('Ctrl Pts',(-0.210285413083626,-0.536155874351713,
-1.09222700315404));
#9017=CARTESIAN_POINT('Ctrl Pts',(-0.233650458981807,-0.890499509100915,
-0.91820429171172));
#9018=CARTESIAN_POINT('Ctrl Pts',(-0.257015504879988,-1.15218247312701,
-0.555833785939323));
#9019=CARTESIAN_POINT('Ctrl Pts',(-0.280380550778169,-1.20561690440758,
-0.164817479243857));
#9020=CARTESIAN_POINT('Ctrl Pts',(-0.283622817135466,-1.21303176931378,
-0.110557837645978));
#9021=CARTESIAN_POINT('Ctrl Pts',(-0.286865083492763,-1.21643661870328,
-0.0557465950131454));
#9022=CARTESIAN_POINT('Ctrl Pts',(-0.29010734985006,-1.21601418463372,-0.00087989446188777));
#9023=CARTESIAN_POINT('Origin',(0.,1.9,3.));
#9024=CARTESIAN_POINT('',(0.,1.9,-1.2051970793194));
#9025=CARTESIAN_POINT('',(1.,1.9,-1.2051970793194));
#9026=CARTESIAN_POINT('',(0.5,1.9,-1.2051970793194));
#9027=CARTESIAN_POINT('',(0.,1.9,1.2051970793194));
#9028=CARTESIAN_POINT('',(0.,1.9,1.5));
#9029=CARTESIAN_POINT('',(1.,1.9,1.2051970793194));
#9030=CARTESIAN_POINT('',(0.5,1.9,1.2051970793194));
#9031=CARTESIAN_POINT('',(1.,1.9,1.5));
#9032=CARTESIAN_POINT('Origin',(0.,-1.9,-3.));
#9033=CARTESIAN_POINT('',(0.,-1.9,1.2051970793194));
#9034=CARTESIAN_POINT('',(1.,-1.9,1.2051970793194));
#9035=CARTESIAN_POINT('',(0.5,-1.9,1.2051970793194));
#9036=CARTESIAN_POINT('',(0.,-1.9,-1.2051970793194));
#9037=CARTESIAN_POINT('',(0.,-1.9,-1.5));
#9038=CARTESIAN_POINT('',(1.,-1.9,-1.2051970793194));
#9039=CARTESIAN_POINT('',(0.5,-1.9,-1.2051970793194));
#9040=CARTESIAN_POINT('',(1.,-1.9,-1.5));
#9041=CARTESIAN_POINT('Origin',(1.,1.5,0.));
#9042=CARTESIAN_POINT('Origin',(1.,0.,0.));
#9043=CARTESIAN_POINT('Origin',(1.,0.,0.));
#9044=CARTESIAN_POINT('',(1.,-1.5,-1.83697019872103E-16));
#9045=CARTESIAN_POINT('Origin',(1.,0.,0.));
#9046=CARTESIAN_POINT('Origin',(0.5,0.,0.));
#9047=CARTESIAN_POINT('Origin',(0.,0.,0.));
#9048=CARTESIAN_POINT('Origin',(7.15,-1.38777878078145E-16,-0.866025403784439));
#9049=CARTESIAN_POINT('',(7.01007662722764,-1.59086285808736E-16,-0.866025403784439));
#9050=CARTESIAN_POINT('',(7.01007662722764,-0.75,-0.433012701892219));
#9051=CARTESIAN_POINT('Origin',(4.4,-0.375,-0.649519052838329));
#9052=CARTESIAN_POINT('',(5.75,-1.38777878078145E-16,-0.866025403784439));
#9053=CARTESIAN_POINT('',(7.15,-1.59086285808736E-16,-0.866025403784439));
#9054=CARTESIAN_POINT('',(5.75,-0.75,-0.433012701892219));
#9055=CARTESIAN_POINT('',(5.75,-0.75,-0.433012701892219));
#9056=CARTESIAN_POINT('',(7.15,-0.75,-0.433012701892219));
#9057=CARTESIAN_POINT('Origin',(7.15,-0.75,-0.433012701892219));
#9058=CARTESIAN_POINT('',(7.01007662722764,-0.75,0.433012701892219));
#9059=CARTESIAN_POINT('Origin',(4.4,-0.75,-1.20185167898973E-16));
#9060=CARTESIAN_POINT('',(5.75,-0.75,0.433012701892219));
#9061=CARTESIAN_POINT('',(5.75,-0.75,0.433012701892219));
#9062=CARTESIAN_POINT('',(7.15,-0.75,0.433012701892219));
#9063=CARTESIAN_POINT('Origin',(7.15,-0.75,0.433012701892219));
#9064=CARTESIAN_POINT('',(7.01007662722764,5.30287619362454E-17,0.866025403784439));
#9065=CARTESIAN_POINT('Origin',(4.4,-0.375,0.649519052838329));
#9066=CARTESIAN_POINT('',(5.75,0.,0.866025403784439));
#9067=CARTESIAN_POINT('',(5.75,5.30287619362453E-17,0.866025403784439));
#9068=CARTESIAN_POINT('',(7.15,5.30287619362453E-17,0.866025403784439));
#9069=CARTESIAN_POINT('Origin',(7.15,0.,0.866025403784439));
#9070=CARTESIAN_POINT('',(7.01007662722764,0.75,0.433012701892219));
#9071=CARTESIAN_POINT('Origin',(4.4,0.375,0.649519052838329));
#9072=CARTESIAN_POINT('',(5.75,0.75,0.433012701892219));
#9073=CARTESIAN_POINT('',(5.75,0.75,0.433012701892219));
#9074=CARTESIAN_POINT('',(7.15,0.75,0.433012701892219));
#9075=CARTESIAN_POINT('Origin',(7.15,0.75,-0.43301270189222));
#9076=CARTESIAN_POINT('',(7.01007662722764,0.75,-0.43301270189222));
#9077=CARTESIAN_POINT('Origin',(4.4,0.375,-0.649519052838329));
#9078=CARTESIAN_POINT('',(5.75,0.75,-0.43301270189222));
#9079=CARTESIAN_POINT('',(7.15,0.75,-0.43301270189222));
#9080=CARTESIAN_POINT('',(5.75,-1.59086285808736E-16,-0.866025403784439));
#9081=CARTESIAN_POINT('Origin',(7.15,0.75,0.433012701892219));
#9082=CARTESIAN_POINT('Origin',(4.4,0.75,-2.40370335797945E-16));
#9083=CARTESIAN_POINT('',(5.75,0.75,-0.43301270189222));
#9084=CARTESIAN_POINT('Origin',(5.75,0.,0.));
#9085=CARTESIAN_POINT('Origin',(4.4,-2.77555756156289E-16,0.));
#9086=CARTESIAN_POINT('',(2.09511388567678,-1.5,1.83697019872103E-16));
#9087=CARTESIAN_POINT('',(2.09511388567678,-5.59822896386801E-16,1.5));
#9088=CARTESIAN_POINT('Origin',(2.09511388567678,0.,0.));
#9089=CARTESIAN_POINT('',(2.09511388567678,-5.59822896386801E-16,-1.5));
#9090=CARTESIAN_POINT('Origin',(2.09511388567678,0.,0.));
#9091=CARTESIAN_POINT('',(4.4,-2.77555756156289E-16,-2.75));
#9092=CARTESIAN_POINT('Origin',(4.4,-2.77555756156289E-16,0.));
#9093=CARTESIAN_POINT('Origin',(2.09511388567678,0.,0.));
#9094=CARTESIAN_POINT('',(4.4,-2.77555756156289E-16,2.75));
#9095=CARTESIAN_POINT('Origin',(4.4,-2.77555756156289E-16,0.));
#9096=CARTESIAN_POINT('Origin',(-2.4,1.05,0.));
#9097=CARTESIAN_POINT('',(-2.4,-1.05,-1.28587913910472E-16));
#9098=CARTESIAN_POINT('Origin',(-2.4,0.,0.));
#9099=CARTESIAN_POINT('Origin',(-2.3,0.,0.));
#9100=CARTESIAN_POINT('',(-2.3,-1.15,-1.40834381901946E-16));
#9101=CARTESIAN_POINT('Origin',(-1.1,0.,0.));
#9102=CARTESIAN_POINT('Origin',(0.,0.,0.));
#9103=CARTESIAN_POINT('Origin',(0.,2.25,0.));
#9104=CARTESIAN_POINT('Origin',(0.,0.,0.));
#9105=CARTESIAN_POINT('Origin',(0.5,0.,0.));
#9106=CARTESIAN_POINT('Origin',(1.74755694283839,0.,0.));
#9107=CARTESIAN_POINT('',(1.74755694283839,-1.5,-1.83697019872103E-16));
#9108=CARTESIAN_POINT('',(0.,0.,0.));
#9109=CARTESIAN_POINT('Origin',(23.9292893218813,0.,-6.86237372364135E-17));
#9110=CARTESIAN_POINT('',(24.,1.9,-2.32682891837997E-16));
#9111=CARTESIAN_POINT('Origin',(24.,0.,0.));
#9112=CARTESIAN_POINT('',(23.8585786437627,2.24142135623731,2.74494948945654E-16));
#9113=CARTESIAN_POINT('',(23.9292893218813,2.07071067811866,2.53588920391826E-16));
#9114=CARTESIAN_POINT('',(23.8585786437627,-2.24142135623731,-2.74494948945654E-16));
#9115=CARTESIAN_POINT('Origin',(23.8585786437627,0.,-1.37247474472827E-16));
#9116=CARTESIAN_POINT('Origin',(23.8585786437627,0.,-1.37247474472827E-16));
#9117=CARTESIAN_POINT('Origin',(23.8,0.,0.));
#9118=CARTESIAN_POINT('',(23.6,-2.5,-3.06161699786838E-16));
#9119=CARTESIAN_POINT('',(23.8,-2.3,-2.81668763803891E-16));
#9120=CARTESIAN_POINT('Origin',(23.6,0.,0.));
#9121=CARTESIAN_POINT('Origin',(24.,0.,0.));
#9122=CARTESIAN_POINT('Origin',(-13.9292893218813,0.,-6.86237372364135E-17));
#9123=CARTESIAN_POINT('',(-13.8585786437627,2.24142135623731,-2.74494948945654E-16));
#9124=CARTESIAN_POINT('',(-13.8585786437627,-2.24142135623731,-2.74494948945654E-16));
#9125=CARTESIAN_POINT('Origin',(-13.8585786437627,0.,-1.37247474472827E-16));
#9126=CARTESIAN_POINT('Origin',(-13.8585786437627,0.,-1.37247474472827E-16));
#9127=CARTESIAN_POINT('',(-14.,1.9,2.32682891837997E-16));
#9128=CARTESIAN_POINT('',(-13.9292893218813,2.07071067811866,2.53588920391826E-16));
#9129=CARTESIAN_POINT('Origin',(-14.,0.,0.));
#9130=CARTESIAN_POINT('Origin',(-14.,2.1,0.));
#9131=CARTESIAN_POINT('Origin',(-13.8,0.,0.));
#9132=CARTESIAN_POINT('',(-13.6,-2.5,-3.06161699786838E-16));
#9133=CARTESIAN_POINT('Origin',(-13.6,0.,0.));
#9134=CARTESIAN_POINT('',(-13.8,-2.3,-2.81668763803891E-16));
#9135=CARTESIAN_POINT('Origin',(20.,0.,3.));
#9136=CARTESIAN_POINT('',(20.,0.800000000000001,2.3685438564654));
#9137=CARTESIAN_POINT('',(19.2,9.79717439317883E-17,2.5));
#9138=CARTESIAN_POINT('Ctrl Pts',(20.,0.800000000000001,2.3685438564654));
#9139=CARTESIAN_POINT('Ctrl Pts',(20.10124341178,0.800000000000001,2.3685438564654));
#9140=CARTESIAN_POINT('Ctrl Pts',(20.2087021071075,0.779619973172144,2.37571629748165));
#9141=CARTESIAN_POINT('Ctrl Pts',(20.4055671254356,0.697767352464298,2.40103225043771));
#9142=CARTESIAN_POINT('Ctrl Pts',(20.4950422069344,0.63632864296403,2.41874877205569));
#9143=CARTESIAN_POINT('Ctrl Pts',(20.6363010586268,0.495069791271689,2.45156308488026));
#9144=CARTESIAN_POINT('Ctrl Pts',(20.697761056251,0.405583630634407,2.46887493070887));
#9145=CARTESIAN_POINT('Ctrl Pts',(20.7796294856729,0.208677866314441,2.49324989776594));
#9146=CARTESIAN_POINT('Ctrl Pts',(20.8,0.101203878863841,2.5));
#9147=CARTESIAN_POINT('Ctrl Pts',(20.8,-0.101203878863841,2.5));
#9148=CARTESIAN_POINT('Ctrl Pts',(20.7796294856729,-0.208677866314441,2.49324989776594));
#9149=CARTESIAN_POINT('Ctrl Pts',(20.697761056251,-0.405583630634407,2.46887493070887));
#9150=CARTESIAN_POINT('Ctrl Pts',(20.6363010586268,-0.495069791271689,2.45156308488026));
#9151=CARTESIAN_POINT('Ctrl Pts',(20.4950422069344,-0.63632864296403,2.41874877205569));
#9152=CARTESIAN_POINT('Ctrl Pts',(20.4055671254356,-0.697767352464298,2.40103225043771));
#9153=CARTESIAN_POINT('Ctrl Pts',(20.2087021071075,-0.779619973172144,2.37571629748165));
#9154=CARTESIAN_POINT('Ctrl Pts',(20.10124341178,-0.800000000000001,2.3685438564654));
#9155=CARTESIAN_POINT('Ctrl Pts',(19.89875658822,-0.800000000000001,2.3685438564654));
#9156=CARTESIAN_POINT('Ctrl Pts',(19.7912978928925,-0.779619973172145,2.37571629748165));
#9157=CARTESIAN_POINT('Ctrl Pts',(19.5944328745644,-0.697767352464302,2.40103225043771));
#9158=CARTESIAN_POINT('Ctrl Pts',(19.5049577930656,-0.636328642964029,2.41874877205569));
#9159=CARTESIAN_POINT('Ctrl Pts',(19.3636989413732,-0.495069791271689,2.45156308488026));
#9160=CARTESIAN_POINT('Ctrl Pts',(19.302238943749,-0.405583630634409,2.46887493070887));
#9161=CARTESIAN_POINT('Ctrl Pts',(19.2203705143271,-0.208677866314441,2.49324989776594));
#9162=CARTESIAN_POINT('Ctrl Pts',(19.2,-0.101203878863841,2.5));
#9163=CARTESIAN_POINT('Ctrl Pts',(19.2,-6.93889390390723E-17,2.5));
#9164=CARTESIAN_POINT('Ctrl Pts',(19.2,-1.21430643318376E-16,2.5));
#9165=CARTESIAN_POINT('Ctrl Pts',(19.2,0.101203878863841,2.5));
#9166=CARTESIAN_POINT('Ctrl Pts',(19.2203705143271,0.208677866314441,2.49324989776594));
#9167=CARTESIAN_POINT('Ctrl Pts',(19.302238943749,0.405583630634408,2.46887493070887));
#9168=CARTESIAN_POINT('Ctrl Pts',(19.3636989413732,0.495069791271689,2.45156308488026));
#9169=CARTESIAN_POINT('Ctrl Pts',(19.5049577930656,0.636328642964029,2.41874877205569));
#9170=CARTESIAN_POINT('Ctrl Pts',(19.5944328745644,0.697767352464302,2.40103225043771));
#9171=CARTESIAN_POINT('Ctrl Pts',(19.7912978928925,0.779619973172145,2.37571629748165));
#9172=CARTESIAN_POINT('Ctrl Pts',(19.89875658822,0.800000000000001,2.3685438564654));
#9173=CARTESIAN_POINT('Ctrl Pts',(20.,0.800000000000001,2.3685438564654));
#9174=CARTESIAN_POINT('',(19.2,9.79717439317883E-17,-2.5));
#9175=CARTESIAN_POINT('',(19.2,9.79717439317883E-17,3.));
#9176=CARTESIAN_POINT('',(20.,0.800000000000001,-2.3685438564654));
#9177=CARTESIAN_POINT('Ctrl Pts',(20.,0.800000000000001,-2.3685438564654));
#9178=CARTESIAN_POINT('Ctrl Pts',(19.89875658822,0.800000000000001,-2.3685438564654));
#9179=CARTESIAN_POINT('Ctrl Pts',(19.7912978928925,0.779619973172145,-2.37571629748165));
#9180=CARTESIAN_POINT('Ctrl Pts',(19.5944328745644,0.697767352464302,-2.40103225043771));
#9181=CARTESIAN_POINT('Ctrl Pts',(19.5049577930656,0.636328642964029,-2.41874877205569));
#9182=CARTESIAN_POINT('Ctrl Pts',(19.3636989413732,0.495069791271689,-2.45156308488026));
#9183=CARTESIAN_POINT('Ctrl Pts',(19.302238943749,0.405583630634408,-2.46887493070887));
#9184=CARTESIAN_POINT('Ctrl Pts',(19.2203705143271,0.208677866314441,-2.49324989776594));
#9185=CARTESIAN_POINT('Ctrl Pts',(19.2,0.101203878863841,-2.5));
#9186=CARTESIAN_POINT('Ctrl Pts',(19.2,-1.73472347597681E-17,-2.5));
#9187=CARTESIAN_POINT('Ctrl Pts',(19.2,-2.16840434497101E-16,-2.5));
#9188=CARTESIAN_POINT('Ctrl Pts',(19.2,-0.101203878863841,-2.5));
#9189=CARTESIAN_POINT('Ctrl Pts',(19.2203705143271,-0.208677866314441,-2.49324989776594));
#9190=CARTESIAN_POINT('Ctrl Pts',(19.302238943749,-0.405583630634408,-2.46887493070887));
#9191=CARTESIAN_POINT('Ctrl Pts',(19.3636989413732,-0.495069791271689,-2.45156308488026));
#9192=CARTESIAN_POINT('Ctrl Pts',(19.5049577930656,-0.636328642964029,-2.41874877205569));
#9193=CARTESIAN_POINT('Ctrl Pts',(19.5944328745644,-0.697767352464302,-2.40103225043771));
#9194=CARTESIAN_POINT('Ctrl Pts',(19.7912978928925,-0.779619973172145,-2.37571629748165));
#9195=CARTESIAN_POINT('Ctrl Pts',(19.89875658822,-0.800000000000001,-2.3685438564654));
#9196=CARTESIAN_POINT('Ctrl Pts',(20.10124341178,-0.800000000000001,-2.3685438564654));
#9197=CARTESIAN_POINT('Ctrl Pts',(20.2087021071075,-0.779619973172144,-2.37571629748165));
#9198=CARTESIAN_POINT('Ctrl Pts',(20.4055671254356,-0.697767352464298,-2.40103225043771));
#9199=CARTESIAN_POINT('Ctrl Pts',(20.4950422069344,-0.63632864296403,-2.41874877205569));
#9200=CARTESIAN_POINT('Ctrl Pts',(20.6363010586268,-0.495069791271689,-2.45156308488026));
#9201=CARTESIAN_POINT('Ctrl Pts',(20.697761056251,-0.405583630634407,-2.46887493070887));
#9202=CARTESIAN_POINT('Ctrl Pts',(20.7796294856729,-0.208677866314441,-2.49324989776594));
#9203=CARTESIAN_POINT('Ctrl Pts',(20.8,-0.101203878863841,-2.5));
#9204=CARTESIAN_POINT('Ctrl Pts',(20.8,0.101203878863841,-2.5));
#9205=CARTESIAN_POINT('Ctrl Pts',(20.7796294856729,0.208677866314441,-2.49324989776594));
#9206=CARTESIAN_POINT('Ctrl Pts',(20.697761056251,0.405583630634407,-2.46887493070887));
#9207=CARTESIAN_POINT('Ctrl Pts',(20.6363010586268,0.495069791271689,-2.45156308488026));
#9208=CARTESIAN_POINT('Ctrl Pts',(20.4950422069344,0.63632864296403,-2.41874877205569));
#9209=CARTESIAN_POINT('Ctrl Pts',(20.4055671254356,0.697767352464298,-2.40103225043771));
#9210=CARTESIAN_POINT('Ctrl Pts',(20.2087021071075,0.779619973172144,-2.37571629748165));
#9211=CARTESIAN_POINT('Ctrl Pts',(20.10124341178,0.8,-2.3685438564654));
#9212=CARTESIAN_POINT('Ctrl Pts',(20.,0.8,-2.3685438564654));
#9213=CARTESIAN_POINT('Origin',(5.,0.,0.));
#9214=CARTESIAN_POINT('',(5.,-2.5,-3.06161699786838E-16));
#9215=CARTESIAN_POINT('',(0.,0.,0.));
#9216=CARTESIAN_POINT('Origin',(19.88,-2.88,7.));
#9217=CARTESIAN_POINT('',(20.,-2.76,8.6));
#9218=CARTESIAN_POINT('',(19.76,-3.,8.6));
#9219=CARTESIAN_POINT('',(20.,-2.76,8.6));
#9220=CARTESIAN_POINT('',(19.76,-3.,-2.35034248182107));
#9221=CARTESIAN_POINT('',(19.76,-3.,7.));
#9222=CARTESIAN_POINT('',(20.,-2.76,-2.35034248182107));
#9223=CARTESIAN_POINT('',(19.76,-3.,-2.35034248182107));
#9224=CARTESIAN_POINT('',(20.,-2.76,7.));
#9225=CARTESIAN_POINT('Origin',(19.2,-2.88,8.6));
#9226=CARTESIAN_POINT('',(19.2,-2.76,9.4));
#9227=CARTESIAN_POINT('Origin',(19.2,-2.76,8.6));
#9228=CARTESIAN_POINT('',(19.2,-3.,9.16));
#9229=CARTESIAN_POINT('',(19.2,-2.76,9.4));
#9230=CARTESIAN_POINT('Origin',(19.2,-3.,8.6));
#9231=CARTESIAN_POINT('Origin',(13.25,-2.88,9.28));
#9232=CARTESIAN_POINT('',(12.,-2.76,9.4));
#9233=CARTESIAN_POINT('',(13.25,-2.76,9.4));
#9234=CARTESIAN_POINT('',(12.,-3.,9.16));
#9235=CARTESIAN_POINT('',(12.,-2.76,9.4));
#9236=CARTESIAN_POINT('',(13.25,-3.,9.16));
#9237=CARTESIAN_POINT('Origin',(12.,0.,9.28));
#9238=CARTESIAN_POINT('',(12.,2.76,9.4));
#9239=CARTESIAN_POINT('Origin',(12.,0.,9.4));
#9240=CARTESIAN_POINT('',(12.,3.,9.16));
#9241=CARTESIAN_POINT('',(12.,2.76,9.4));
#9242=CARTESIAN_POINT('Origin',(12.,0.,9.16));
#9243=CARTESIAN_POINT('Origin',(17.25,2.88,9.28));
#9244=CARTESIAN_POINT('',(19.2,2.76,9.4));
#9245=CARTESIAN_POINT('',(17.25,2.76,9.4));
#9246=CARTESIAN_POINT('',(19.2,3.,9.16));
#9247=CARTESIAN_POINT('',(19.2,2.76,9.4));
#9248=CARTESIAN_POINT('',(17.25,3.,9.16));
#9249=CARTESIAN_POINT('Origin',(19.2,2.88,8.6));
#9250=CARTESIAN_POINT('',(20.,2.76,8.6));
#9251=CARTESIAN_POINT('Origin',(19.2,2.76,8.6));
#9252=CARTESIAN_POINT('',(19.76,3.,8.6));
#9253=CARTESIAN_POINT('',(20.,2.76,8.6));
#9254=CARTESIAN_POINT('Origin',(19.2,3.,8.6));
#9255=CARTESIAN_POINT('Origin',(19.88,2.88,7.));
#9256=CARTESIAN_POINT('',(20.,2.76,-2.35034248182107));
#9257=CARTESIAN_POINT('',(19.76,3.,-2.35034248182107));
#9258=CARTESIAN_POINT('',(20.,2.76,-2.35034248182107));
#9259=CARTESIAN_POINT('',(19.76,3.,7.));
#9260=CARTESIAN_POINT('',(20.,2.76,7.));
#9261=CARTESIAN_POINT('Origin',(20.8,2.88,-2.35034248182107));
#9262=CARTESIAN_POINT('',(20.3130434782609,2.76,-2.98506552846088));
#9263=CARTESIAN_POINT('Origin',(20.8,2.76,-2.35034248182107));
#9264=CARTESIAN_POINT('',(20.1669565217391,3.,-3.17548244245282));
#9265=CARTESIAN_POINT('',(20.3130434782609,2.76,-2.98506552846088));
#9266=CARTESIAN_POINT('Origin',(20.8,3.,-2.35034248182107));
#9267=CARTESIAN_POINT('Origin',(18.,2.88,-6.));
#9268=CARTESIAN_POINT('',(15.6869565217391,2.76,-2.98506552846088));
#9269=CARTESIAN_POINT('',(15.8330434782609,3.,-3.17548244245283));
#9270=CARTESIAN_POINT('',(15.6869565217391,2.76,-2.98506552846088));
#9271=CARTESIAN_POINT('Origin',(18.,3.,-6.));
#9272=CARTESIAN_POINT('Origin',(18.,2.76,-6.));
#9273=CARTESIAN_POINT('Origin',(15.2,2.88,-2.35034248182107));
#9274=CARTESIAN_POINT('',(16.,2.76,-2.35034248182107));
#9275=CARTESIAN_POINT('Origin',(15.2,2.76,-2.35034248182107));
#9276=CARTESIAN_POINT('',(16.24,3.,-2.35034248182107));
#9277=CARTESIAN_POINT('',(16.,2.76,-2.35034248182107));
#9278=CARTESIAN_POINT('Origin',(15.2,3.,-2.35034248182107));
#9279=CARTESIAN_POINT('Origin',(16.12,2.88,2.11554944214035));
#9280=CARTESIAN_POINT('',(16.,2.76,6.2));
#9281=CARTESIAN_POINT('',(16.24,3.,6.2));
#9282=CARTESIAN_POINT('',(16.,2.76,6.2));
#9283=CARTESIAN_POINT('',(16.24,3.,2.11554944214035));
#9284=CARTESIAN_POINT('',(16.,2.76,2.11554944214035));
#9285=CARTESIAN_POINT('Origin',(15.2,2.88,6.2));
#9286=CARTESIAN_POINT('',(15.2,2.76,7.));
#9287=CARTESIAN_POINT('Origin',(15.2,2.76,6.2));
#9288=CARTESIAN_POINT('',(15.2,3.,7.24));
#9289=CARTESIAN_POINT('',(15.2,2.76,7.));
#9290=CARTESIAN_POINT('Origin',(15.2,3.,6.2));
#9291=CARTESIAN_POINT('Origin',(17.25,2.88,7.12));
#9292=CARTESIAN_POINT('',(12.,2.76,7.));
#9293=CARTESIAN_POINT('',(12.,3.,7.24));
#9294=CARTESIAN_POINT('',(12.,2.76,7.));
#9295=CARTESIAN_POINT('',(17.25,3.,7.24));
#9296=CARTESIAN_POINT('',(17.25,2.76,7.));
#9297=CARTESIAN_POINT('Origin',(12.,0.,7.12));
#9298=CARTESIAN_POINT('',(12.,-2.76,7.));
#9299=CARTESIAN_POINT('',(12.,-3.,7.24));
#9300=CARTESIAN_POINT('',(12.,-2.76,7.));
#9301=CARTESIAN_POINT('Origin',(12.,0.,7.24));
#9302=CARTESIAN_POINT('Origin',(12.,0.,7.));
#9303=CARTESIAN_POINT('Origin',(13.25,-2.88,7.12));
#9304=CARTESIAN_POINT('',(15.2,-2.76,7.));
#9305=CARTESIAN_POINT('',(15.2,-3.,7.24));
#9306=CARTESIAN_POINT('',(15.2,-2.76,7.));
#9307=CARTESIAN_POINT('',(13.25,-3.,7.24));
#9308=CARTESIAN_POINT('',(13.25,-2.76,7.));
#9309=CARTESIAN_POINT('Origin',(15.2,-2.88,6.2));
#9310=CARTESIAN_POINT('',(16.,-2.76,6.2));
#9311=CARTESIAN_POINT('Origin',(15.2,-2.76,6.2));
#9312=CARTESIAN_POINT('',(16.24,-3.,6.2));
#9313=CARTESIAN_POINT('',(16.,-2.76,6.2));
#9314=CARTESIAN_POINT('Origin',(15.2,-3.,6.2));
#9315=CARTESIAN_POINT('Origin',(16.12,-2.88,2.11554944214035));
#9316=CARTESIAN_POINT('',(16.,-2.76,-2.35034248182107));
#9317=CARTESIAN_POINT('',(16.,-2.76,2.11554944214035));
#9318=CARTESIAN_POINT('',(16.24,-3.,-2.35034248182107));
#9319=CARTESIAN_POINT('',(16.,-2.76,-2.35034248182107));
#9320=CARTESIAN_POINT('',(16.24,-3.,2.11554944214035));
#9321=CARTESIAN_POINT('Origin',(15.2,-2.88,-2.35034248182107));
#9322=CARTESIAN_POINT('',(15.6869565217391,-2.76,-2.98506552846088));
#9323=CARTESIAN_POINT('Origin',(15.2,-2.76,-2.35034248182107));
#9324=CARTESIAN_POINT('',(15.8330434782609,-3.,-3.17548244245283));
#9325=CARTESIAN_POINT('',(15.6869565217391,-2.76,-2.98506552846088));
#9326=CARTESIAN_POINT('Origin',(15.2,-3.,-2.35034248182107));
#9327=CARTESIAN_POINT('Origin',(18.,-2.88,-6.));
#9328=CARTESIAN_POINT('',(20.3130434782609,-2.76,-2.98506552846088));
#9329=CARTESIAN_POINT('Origin',(18.,-2.76,-6.));
#9330=CARTESIAN_POINT('',(20.1669565217391,-3.,-3.17548244245283));
#9331=CARTESIAN_POINT('',(20.3130434782609,-2.76,-2.98506552846088));
#9332=CARTESIAN_POINT('Origin',(18.,-3.,-6.));
#9333=CARTESIAN_POINT('Origin',(20.8,-2.88,-2.35034248182107));
#9334=CARTESIAN_POINT('Origin',(20.8,-2.76,-2.35034248182107));
#9335=CARTESIAN_POINT('Origin',(20.8,-3.,-2.35034248182107));
#9336=CARTESIAN_POINT('Origin',(14.5,0.,9.4));
#9337=CARTESIAN_POINT('',(19.2,-1.5,9.4));
#9338=CARTESIAN_POINT('',(10.95,-1.28587913910472E-16,9.4));
#9339=CARTESIAN_POINT('Origin',(12.,0.,9.4));
#9340=CARTESIAN_POINT('Origin',(15.2,-3.,-2.35034248182107));
#9341=CARTESIAN_POINT('',(15.6869565217391,-3.,-2.98506552846088));
#9342=CARTESIAN_POINT('',(16.,-3.,-2.35034248182107));
#9343=CARTESIAN_POINT('Origin',(18.,-3.,-6.));
#9344=CARTESIAN_POINT('',(20.3130434782609,-3.,-2.98506552846088));
#9345=CARTESIAN_POINT('Origin',(19.2,-1.5,8.6));
#9346=CARTESIAN_POINT('',(20.,-1.5,8.6));
#9347=CARTESIAN_POINT('Origin',(20.8,-3.,-2.35034248182107));
#9348=CARTESIAN_POINT('',(20.,-3.,-2.35034248182107));
#9349=CARTESIAN_POINT('Origin',(20.,-3.,7.));
#9350=CARTESIAN_POINT('Origin',(12.,-3.,7.));
#9351=CARTESIAN_POINT('',(12.,-3.,7.));
#9352=CARTESIAN_POINT('',(15.99,-3.,-6.));
#9353=CARTESIAN_POINT('Origin',(18.,-3.,-6.));
#9354=CARTESIAN_POINT('Origin',(12.,0.,7.));
#9355=CARTESIAN_POINT('',(12.,3.,7.));
#9356=CARTESIAN_POINT('Origin',(16.,-3.,-2.7689011157193));
#9357=CARTESIAN_POINT('',(16.,-1.5,6.2));
#9358=CARTESIAN_POINT('Origin',(15.2,-1.5,6.2));
#9359=CARTESIAN_POINT('',(15.2,-1.5,7.));
#9360=CARTESIAN_POINT('Origin',(18.,-3.,-6.));
#9361=CARTESIAN_POINT('',(15.99,3.,-6.));
#9362=CARTESIAN_POINT('',(15.99,-3.,-6.));
#9363=CARTESIAN_POINT('Origin',(18.,3.,-6.));
#9364=CARTESIAN_POINT('Origin',(12.,0.,9.4));
#9365=CARTESIAN_POINT('',(10.95,-1.28587913910472E-16,7.));
#9366=CARTESIAN_POINT('',(10.95,1.28587913910472E-16,9.4));
#9367=CARTESIAN_POINT('Origin',(12.,0.,7.));
#9368=CARTESIAN_POINT('Origin',(20.,3.,7.));
#9369=CARTESIAN_POINT('Origin',(14.5,0.,7.));
#9370=CARTESIAN_POINT('',(0.,0.,0.));
#9371=CARTESIAN_POINT('Origin',(1.55,0.,0.));
#9372=CARTESIAN_POINT('',(3.1,-1.05,-1.28587913910472E-16));
#9373=CARTESIAN_POINT('Origin',(3.1,0.,0.));
#9374=CARTESIAN_POINT('',(0.,-1.05,-1.28587913910472E-16));
#9375=CARTESIAN_POINT('',(1.55,-1.05,-1.28587913910472E-16));
#9376=CARTESIAN_POINT('Origin',(0.,0.,0.));
#9377=CARTESIAN_POINT('Origin',(0.,1.5,0.));
#9378=CARTESIAN_POINT('',(0.,-1.5,-1.83697019872103E-16));
#9379=CARTESIAN_POINT('Origin',(0.,0.,0.));
#9380=CARTESIAN_POINT('Origin',(1.3,0.,0.));
#9381=CARTESIAN_POINT('',(2.6,-1.5,-1.83697019872103E-16));
#9382=CARTESIAN_POINT('Origin',(2.6,0.,0.));
#9383=CARTESIAN_POINT('',(1.3,-1.5,-1.83697019872103E-16));
#9384=CARTESIAN_POINT('Origin',(2.6,2.25,0.));
#9385=CARTESIAN_POINT('',(2.6,-2.25,-2.75545529808154E-16));
#9386=CARTESIAN_POINT('Origin',(2.6,0.,0.));
#9387=CARTESIAN_POINT('Origin',(2.85,0.,0.));
#9388=CARTESIAN_POINT('',(3.1,-2.25,-2.75545529808154E-16));
#9389=CARTESIAN_POINT('Origin',(3.1,0.,0.));
#9390=CARTESIAN_POINT('',(2.85,-2.25,-2.75545529808154E-16));
#9391=CARTESIAN_POINT('Origin',(3.1,1.05,0.));
#9392=CARTESIAN_POINT('',(0.,0.,0.));
#9393=CARTESIAN_POINT('Origin',(-2.4,0.,0.));
#9394=CARTESIAN_POINT('',(-4.70426408311032,-0.96799663351158,0.000586579696609281));
#9395=CARTESIAN_POINT('',(-4.76223591688968,-0.967694506288088,0.00103882260809823));
#9396=CARTESIAN_POINT('',(-2.4,-0.96675,-1.1839272930757E-16));
#9397=CARTESIAN_POINT('',(-4.83325,0.425622480653816,0.868929115424972));
#9398=CARTESIAN_POINT('Ctrl Pts',(-4.70426408311032,-0.96799663351158,0.000586579696609281));
#9399=CARTESIAN_POINT('Ctrl Pts',(-4.70622252020084,-0.968188696529655,
0.0302155518677432));
#9400=CARTESIAN_POINT('Ctrl Pts',(-4.70818095729136,-0.96694718755688,0.0598270303413266));
#9401=CARTESIAN_POINT('Ctrl Pts',(-4.71013939438189,-0.964219781588607,
0.0892995654647602));
#9402=CARTESIAN_POINT('Ctrl Pts',(-4.73135623850072,-0.934672267625714,
0.408592018884498));
#9403=CARTESIAN_POINT('Ctrl Pts',(-4.75257308261956,-0.730730960219766,
0.711577246447129));
#9404=CARTESIAN_POINT('Ctrl Pts',(-4.7737899267384,-0.446054125841313,0.85939924826032));
#9405=CARTESIAN_POINT('Ctrl Pts',(-4.79360995115893,-0.180119108468427,
0.997489327511466));
#9406=CARTESIAN_POINT('Ctrl Pts',(-4.81342997557947,0.156270854454437,1.00017412693755));
#9407=CARTESIAN_POINT('Ctrl Pts',(-4.83325,0.426125832792548,0.869596007169463));
#9408=CARTESIAN_POINT('',(-4.83325,-0.425119128515146,0.868262223680452));
#9409=CARTESIAN_POINT('Origin',(-4.83325,0.,0.));
#9410=CARTESIAN_POINT('Ctrl Pts',(-4.83325,-0.425119128515143,0.868262223680453));
#9411=CARTESIAN_POINT('Ctrl Pts',(-4.81203315588116,-0.714487838908671,
0.726581322880003));
#9412=CARTESIAN_POINT('Ctrl Pts',(-4.79081631176232,-0.924920061329283,
0.430079065651513));
#9413=CARTESIAN_POINT('Ctrl Pts',(-4.76959946764349,-0.961775931984156,
0.112039025697822));
#9414=CARTESIAN_POINT('Ctrl Pts',(-4.76714495072555,-0.966039683819298,
0.0752458695491139));
#9415=CARTESIAN_POINT('Ctrl Pts',(-4.76469043380762,-0.9679803723504,0.038164461964134));
#9416=CARTESIAN_POINT('Ctrl Pts',(-4.76223591688968,-0.967694506288088,
0.00103882260809823));
#9417=CARTESIAN_POINT('Origin',(-2.4,0.,0.));
#9418=CARTESIAN_POINT('',(-4.30426408311032,-0.965537613432151,0.000605435635551502));
#9419=CARTESIAN_POINT('',(-4.36223591688968,-0.965404024556207,0.000513315930580149));
#9420=CARTESIAN_POINT('',(-2.4,-0.96675,-1.1839272930757E-16));
#9421=CARTESIAN_POINT('Ctrl Pts',(-4.30426408311032,-0.965537613432151,
0.000605435635551502));
#9422=CARTESIAN_POINT('Ctrl Pts',(-4.31225478882116,-0.966229595136308,
0.122298513524397));
#9423=CARTESIAN_POINT('Ctrl Pts',(-4.32024549453199,-0.94492006611068,0.243757898774464));
#9424=CARTESIAN_POINT('Ctrl Pts',(-4.32823620024282,-0.900505236276788,
0.356080422219802));
#9425=CARTESIAN_POINT('Ctrl Pts',(-4.34945304436166,-0.782575411896814,
0.654318094487466));
#9426=CARTESIAN_POINT('Ctrl Pts',(-4.37066988848049,-0.501752398588181,
0.888140567467159));
#9427=CARTESIAN_POINT('Ctrl Pts',(-4.39188673259933,-0.187086076027208,
0.950103612041012));
#9428=CARTESIAN_POINT('Ctrl Pts',(-4.41310357671816,0.127580246533763,1.01206665661487));
#9429=CARTESIAN_POINT('Ctrl Pts',(-4.434320420837,0.476089878347074,0.902170272782879));
#9430=CARTESIAN_POINT('Ctrl Pts',(-4.45553726495584,0.698283934632795,0.670901670209797));
#9431=CARTESIAN_POINT('Ctrl Pts',(-4.47675410907468,0.920477990918515,0.439633067636716));
#9432=CARTESIAN_POINT('Ctrl Pts',(-4.49797095319351,1.01635647167665,0.0869922463225382));
#9433=CARTESIAN_POINT('Ctrl Pts',(-4.51918779731235,0.941863562195449,-0.224936967419801));
#9434=CARTESIAN_POINT('Ctrl Pts',(-4.54040464143119,0.867370652714251,-0.536866181162142));
#9435=CARTESIAN_POINT('Ctrl Pts',(-4.56162148555003,0.622506352993724,-0.808083787332644));
#9436=CARTESIAN_POINT('Ctrl Pts',(-4.58283832966887,0.319788071489397,-0.914007732585481));
#9437=CARTESIAN_POINT('Ctrl Pts',(-4.6040551737877,0.0170697899850713,-1.01993167783832));
#9438=CARTESIAN_POINT('Ctrl Pts',(-4.62527201790654,-0.343502473303055,
-0.960561962173493));
#9439=CARTESIAN_POINT('Ctrl Pts',(-4.64648886202538,-0.596211744687198,
-0.763077264702658));
#9440=CARTESIAN_POINT('Ctrl Pts',(-4.66574726905369,-0.825594492700318,
-0.583821543896356));
#9441=CARTESIAN_POINT('Ctrl Pts',(-4.68500567608201,-0.966107970457212,
-0.290771671566069));
#9442=CARTESIAN_POINT('Ctrl Pts',(-4.70426408311032,-0.96799663351158,0.000586579696609281));
#9443=CARTESIAN_POINT('Ctrl Pts',(-4.76223591688968,-0.967694506288088,
0.00103882260809823));
#9444=CARTESIAN_POINT('Ctrl Pts',(-4.74347358968878,-0.965509346121728,
-0.282749562817477));
#9445=CARTESIAN_POINT('Ctrl Pts',(-4.72471126248788,-0.833224963979337,
-0.569122443147427));
#9446=CARTESIAN_POINT('Ctrl Pts',(-4.70594893528698,-0.613946448276237,
-0.749089767887891));
#9447=CARTESIAN_POINT('Ctrl Pts',(-4.68473209116814,-0.36598157502432,-0.95260069884101));
#9448=CARTESIAN_POINT('Ctrl Pts',(-4.6635152470493,-0.00677230963135718,
-1.02004473806835));
#9449=CARTESIAN_POINT('Ctrl Pts',(-4.64229840293046,0.298368620527852,-0.921144559843448));
#9450=CARTESIAN_POINT('Ctrl Pts',(-4.62108155881162,0.603509550687061,-0.822244381618546));
#9451=CARTESIAN_POINT('Ctrl Pts',(-4.59986471469279,0.854582145612518,-0.556999985941402));
#9452=CARTESIAN_POINT('Ctrl Pts',(-4.57864787057395,0.936330783545615,-0.246938920428587));
#9453=CARTESIAN_POINT('Ctrl Pts',(-4.55743102645511,1.01807942147871,0.0631221450842284));
#9454=CARTESIAN_POINT('Ctrl Pts',(-4.53621418233627,0.93050410241945,0.417999880432715));
#9455=CARTESIAN_POINT('Ctrl Pts',(-4.51499733821743,0.713784719578434,0.654420888771027));
#9456=CARTESIAN_POINT('Ctrl Pts',(-4.4937804940986,0.497065336737419,0.890841897109338));
#9457=CARTESIAN_POINT('Ctrl Pts',(-4.47256364997976,0.151201890114651,1.00880617843748));
#9458=CARTESIAN_POINT('Ctrl Pts',(-4.45134680586093,-0.164831065293702,
0.954203943671648));
#9459=CARTESIAN_POINT('Ctrl Pts',(-4.43012996174209,-0.480864020702056,
0.899601708905819));
#9460=CARTESIAN_POINT('Ctrl Pts',(-4.40891311762325,-0.767066484895994,
0.672432958046022));
#9461=CARTESIAN_POINT('Ctrl Pts',(-4.38769627350441,-0.891933182925361,
0.377039449857775));
#9462=CARTESIAN_POINT('Ctrl Pts',(-4.37920948796617,-0.941880143986509,
0.258881379819561));
#9463=CARTESIAN_POINT('Ctrl Pts',(-4.37072270242792,-0.96601309112653,0.129807225410783));
#9464=CARTESIAN_POINT('Ctrl Pts',(-4.36223591688968,-0.965404024556207,
0.000513315930580149));
#9465=CARTESIAN_POINT('Origin',(-2.4,0.,0.));
#9466=CARTESIAN_POINT('',(-3.90426408311032,-0.965795891256579,-0.000737499302822728));
#9467=CARTESIAN_POINT('',(-3.96223591688968,-0.965982214745567,-0.000801926712228235));
#9468=CARTESIAN_POINT('',(-2.4,-0.96675,-1.1839272930757E-16));
#9469=CARTESIAN_POINT('Ctrl Pts',(-3.90426408311032,-0.965795891256579,
-0.000737499302822728));
#9470=CARTESIAN_POINT('Ctrl Pts',(-3.91828705744146,-0.96428827348378,0.212679227068352));
#9471=CARTESIAN_POINT('Ctrl Pts',(-3.9323100317726,-0.894601612748111,0.426990280137081));
#9472=CARTESIAN_POINT('Ctrl Pts',(-3.94633300610374,-0.764503886089668,
0.594336826719673));
#9473=CARTESIAN_POINT('Ctrl Pts',(-3.96754985022258,-0.567665246757806,
0.847533153606187));
#9474=CARTESIAN_POINT('Ctrl Pts',(-3.98876669434142,-0.232534373605965,
0.99321893729977));
#9475=CARTESIAN_POINT('Ctrl Pts',(-4.00998353846026,0.0868805666510462,
0.964444968964459));
#9476=CARTESIAN_POINT('Ctrl Pts',(-4.03120038257909,0.406295506908058,0.935671000629147));
#9477=CARTESIAN_POINT('Ctrl Pts',(-4.05241722669793,0.709994514270243,0.732437280264936));
#9478=CARTESIAN_POINT('Ctrl Pts',(-4.07363407081677,0.858413740920987,0.448138810550013));
#9479=CARTESIAN_POINT('Ctrl Pts',(-4.09485091493561,1.00683296757173,0.163840340835089));
#9480=CARTESIAN_POINT('Ctrl Pts',(-4.11606775905444,0.999972413511041,-0.201522878230549));
#9481=CARTESIAN_POINT('Ctrl Pts',(-4.13728460317328,0.840984924628371,-0.480048863745562));
#9482=CARTESIAN_POINT('Ctrl Pts',(-4.15850144729212,0.681997435745701,-0.758574849260573));
#9483=CARTESIAN_POINT('Ctrl Pts',(-4.17971829141096,0.370883012041052,-0.950263601224959));
#9484=CARTESIAN_POINT('Ctrl Pts',(-4.20093513552979,0.0506129802060959,
-0.967026417202116));
#9485=CARTESIAN_POINT('Ctrl Pts',(-4.22215197964863,-0.269657051628861,
-0.983789233179273));
#9486=CARTESIAN_POINT('Ctrl Pts',(-4.24336882376746,-0.599082691594126,
-0.825626113169202));
#9487=CARTESIAN_POINT('Ctrl Pts',(-4.2645856678863,-0.786277193851101,-0.56521811738635));
#9488=CARTESIAN_POINT('Ctrl Pts',(-4.27781180629431,-0.902970344924894,
-0.402885200413198));
#9489=CARTESIAN_POINT('Ctrl Pts',(-4.29103794470232,-0.964392252042782,
-0.200819763802405));
#9490=CARTESIAN_POINT('Ctrl Pts',(-4.30426408311032,-0.965537613432151,
0.000605435635551502));
#9491=CARTESIAN_POINT('Ctrl Pts',(-4.36223591688968,-0.965404024556207,
0.000513315930580149));
#9492=CARTESIAN_POINT('Ctrl Pts',(-4.34950585830908,-0.964490433293089,
-0.193425724284307));
#9493=CARTESIAN_POINT('Ctrl Pts',(-4.33677579972849,-0.90790835831582,-0.3878592041094));
#9494=CARTESIAN_POINT('Ctrl Pts',(-4.3240457411479,-0.799275698255333,-0.546688030710467));
#9495=CARTESIAN_POINT('Ctrl Pts',(-4.30282889702907,-0.618220583691147,
-0.811403737573761));
#9496=CARTESIAN_POINT('Ctrl Pts',(-4.28161205291023,-0.29257942269798,-0.977216885783651));
#9497=CARTESIAN_POINT('Ctrl Pts',(-4.26039520879139,0.0279955403970755,
-0.967943309265855));
#9498=CARTESIAN_POINT('Ctrl Pts',(-4.23917836467255,0.348570503492131,-0.958669732748059));
#9499=CARTESIAN_POINT('Ctrl Pts',(-4.21796152055372,0.664079268689074,-0.774309431502578));
#9500=CARTESIAN_POINT('Ctrl Pts',(-4.19674467643488,0.829533552132358,-0.499576789354811));
#9501=CARTESIAN_POINT('Ctrl Pts',(-4.17552783231604,0.994987835575642,-0.224844147207043));
#9502=CARTESIAN_POINT('Ctrl Pts',(-4.1543109881972,1.01038763726526,0.140260835843012));
#9503=CARTESIAN_POINT('Ctrl Pts',(-4.13309414407837,0.868654640976634,0.427951393252367));
#9504=CARTESIAN_POINT('Ctrl Pts',(-4.11187729995953,0.726921644688003,0.715641950661722));
#9505=CARTESIAN_POINT('Ctrl Pts',(-4.09066045584069,0.42805585042112,0.925918082430377));
#9506=CARTESIAN_POINT('Ctrl Pts',(-4.06944361172186,0.109400699885222,0.962150291950837));
#9507=CARTESIAN_POINT('Ctrl Pts',(-4.04822676760302,-0.209254450650673,
0.998382501471297));
#9508=CARTESIAN_POINT('Ctrl Pts',(-4.02700992348418,-0.547698957455582,
0.860570788743565));
#9509=CARTESIAN_POINT('Ctrl Pts',(-4.00579307936534,-0.750402243554795,
0.612044901597546));
#9510=CARTESIAN_POINT('Ctrl Pts',(-3.99127402520679,-0.889115615463787,
0.441974329599889));
#9511=CARTESIAN_POINT('Ctrl Pts',(-3.97675497104823,-0.96426270252421,0.22005739353346));
#9512=CARTESIAN_POINT('Ctrl Pts',(-3.96223591688968,-0.965982214745567,
-0.000801926712228235));
#9513=CARTESIAN_POINT('Origin',(-2.4,0.,0.));
#9514=CARTESIAN_POINT('',(-3.50426408311032,-0.968220991348266,-0.000322423235073616));
#9515=CARTESIAN_POINT('',(-3.56223591688968,-0.968306026645575,-0.000188088405189823));
#9516=CARTESIAN_POINT('',(-2.4,-0.96675,-1.1839272930757E-16));
#9517=CARTESIAN_POINT('Ctrl Pts',(-3.50426408311032,-0.968220991348266,
-0.000322423235073616));
#9518=CARTESIAN_POINT('Ctrl Pts',(-3.52431932606177,-0.966908660198467,
0.302935904290734));
#9519=CARTESIAN_POINT('Ctrl Pts',(-3.54437456901322,-0.812857152984626,
0.607343009605967));
#9520=CARTESIAN_POINT('Ctrl Pts',(-3.56442981196467,-0.567140710421351,
0.784890977004851));
#9521=CARTESIAN_POINT('Ctrl Pts',(-3.58564665608351,-0.307192353180262,
0.972722535916296));
#9522=CARTESIAN_POINT('Ctrl Pts',(-3.60686350020235,0.0553469307636014,
1.0185739966589));
#9523=CARTESIAN_POINT('Ctrl Pts',(-3.62808034432118,0.353873509518189,0.901374487980609));
#9524=CARTESIAN_POINT('Ctrl Pts',(-3.64929718844002,0.652400088272776,0.784174979302323));
#9525=CARTESIAN_POINT('Ctrl Pts',(-3.67051403255886,0.886913961838087,0.503924501203151));
#9526=CARTESIAN_POINT('Ctrl Pts',(-3.69173087667769,0.949645116426769,0.189411152485569));
#9527=CARTESIAN_POINT('Ctrl Pts',(-3.71294772079653,1.01237627101545,-0.125102196232017));
#9528=CARTESIAN_POINT('Ctrl Pts',(-3.73416456491537,0.903324706627501,-0.473878415568014));
#9529=CARTESIAN_POINT('Ctrl Pts',(-3.75538140903421,0.67260468221376,-0.696638626876869));
#9530=CARTESIAN_POINT('Ctrl Pts',(-3.77659825315305,0.441884657800018,-0.919398838185724));
#9531=CARTESIAN_POINT('Ctrl Pts',(-3.79781509727188,0.089496173360486,-1.01614304146744));
#9532=CARTESIAN_POINT('Ctrl Pts',(-3.81903194139072,-0.222621906420323,
-0.942412809037723));
#9533=CARTESIAN_POINT('Ctrl Pts',(-3.84024878550956,-0.534739986201133,
-0.868682576608009));
#9534=CARTESIAN_POINT('Ctrl Pts',(-3.86146562962839,-0.806587661323218,
-0.624477908466866));
#9535=CARTESIAN_POINT('Ctrl Pts',(-3.88268247374723,-0.913238296128317,
-0.322022139356571));
#9536=CARTESIAN_POINT('Ctrl Pts',(-3.88987634353493,-0.949399695781619,
-0.219470251463622));
#9537=CARTESIAN_POINT('Ctrl Pts',(-3.89707021332263,-0.966569308200162,
-0.110221557661356));
#9538=CARTESIAN_POINT('Ctrl Pts',(-3.90426408311032,-0.965795891256579,
-0.000737499302822728));
#9539=CARTESIAN_POINT('Ctrl Pts',(-3.96223591688968,-0.965982214745567,
-0.000801926712228235));
#9540=CARTESIAN_POINT('Ctrl Pts',(-3.9555381269294,-0.96677544353079,-0.102686617107505));
#9541=CARTESIAN_POINT('Ctrl Pts',(-3.94884033696911,-0.951942752824712,
-0.204346239199711));
#9542=CARTESIAN_POINT('Ctrl Pts',(-3.94214254700883,-0.920516057993009,
-0.300587199648137));
#9543=CARTESIAN_POINT('Ctrl Pts',(-3.92092570288999,-0.820964520938493,
-0.60545335218349));
#9544=CARTESIAN_POINT('Ctrl Pts',(-3.89970885877116,-0.554899381435944,
-0.855945595689884));
#9545=CARTESIAN_POINT('Ctrl Pts',(-3.87849201465232,-0.244590031080805,
-0.936951429275862));
#9546=CARTESIAN_POINT('Ctrl Pts',(-3.85727517053348,0.0657193192743316,
-1.01795726286184));
#9547=CARTESIAN_POINT('Ctrl Pts',(-3.83605832641464,0.420272880482055,-0.929476686527402));
#9548=CARTESIAN_POINT('Ctrl Pts',(-3.8148414822958,0.656136887018051,-0.712170467181513));
#9549=CARTESIAN_POINT('Ctrl Pts',(-3.79362463817697,0.892000893554047,-0.494864247835623));
#9550=CARTESIAN_POINT('Ctrl Pts',(-3.77240779405813,1.00917534541831,-0.14873238547828));
#9551=CARTESIAN_POINT('Ctrl Pts',(-3.75119094993929,0.95381311209924,0.167161371971532));
#9552=CARTESIAN_POINT('Ctrl Pts',(-3.72997410582045,0.898450878780169,0.483055129421343));
#9553=CARTESIAN_POINT('Ctrl Pts',(-3.70875726170162,0.670551960277765,0.768710781963624));
#9554=CARTESIAN_POINT('Ctrl Pts',(-3.68754041758278,0.374846505988049,0.892856341236669));
#9555=CARTESIAN_POINT('Ctrl Pts',(-3.66632357346394,0.0791410516983311,
1.01700190050971));
#9556=CARTESIAN_POINT('Ctrl Pts',(-3.64510672934511,-0.284370938378696,
0.979637366513521));
#9557=CARTESIAN_POINT('Ctrl Pts',(-3.62388988522627,-0.548638836403093,
0.797933453061513));
#9558=CARTESIAN_POINT('Ctrl Pts',(-3.60333856244741,-0.804617286448319,
0.621929154089479));
#9559=CARTESIAN_POINT('Ctrl Pts',(-3.58278723966854,-0.967480092264311,
0.310498614343853));
#9560=CARTESIAN_POINT('Ctrl Pts',(-3.56223591688968,-0.968306026645575,
-0.000188088405189823));
#9561=CARTESIAN_POINT('Origin',(-2.4,0.,0.));
#9562=CARTESIAN_POINT('',(-3.10426408311032,-0.966781343451459,0.000892257579201902));
#9563=CARTESIAN_POINT('',(-3.16223591688968,-0.966552838587621,0.000892251240061179));
#9564=CARTESIAN_POINT('',(-2.4,-0.96675,-1.1839272930757E-16));
#9565=CARTESIAN_POINT('Ctrl Pts',(-3.10426408311032,-0.966781343451459,
0.000892257579201902));
#9566=CARTESIAN_POINT('Ctrl Pts',(-3.10913475056325,-0.967466726972738,
0.0748278892399497));
#9567=CARTESIAN_POINT('Ctrl Pts',(-3.11400541801617,-0.959705504164299,
0.14862110473839));
#9568=CARTESIAN_POINT('Ctrl Pts',(-3.11887608546909,-0.942955010012067,
0.220314047443942));
#9569=CARTESIAN_POINT('Ctrl Pts',(-3.14009292958793,-0.869989112262627,
0.532611695457657));
#9570=CARTESIAN_POINT('Ctrl Pts',(-3.16130977370676,-0.626450679734538,
0.805056407642833));
#9571=CARTESIAN_POINT('Ctrl Pts',(-3.1825266178256,-0.324256928886395,0.912447189978175));
#9572=CARTESIAN_POINT('Ctrl Pts',(-3.20374346194444,-0.0220631780382503,
1.01983797231352));
#9573=CARTESIAN_POINT('Ctrl Pts',(-3.22496030606328,0.338785891129949,0.962174824799022));
#9574=CARTESIAN_POINT('Ctrl Pts',(-3.24617715018211,0.592463378288448,0.765956640910963));
#9575=CARTESIAN_POINT('Ctrl Pts',(-3.26739399430095,0.846140865446948,0.569738457022904));
#9576=CARTESIAN_POINT('Ctrl Pts',(-3.28861083841979,0.992646770595747,0.234965236761276));
#9577=CARTESIAN_POINT('Ctrl Pts',(-3.30982768253862,0.964654828496803,-0.0845191828714919));
#9578=CARTESIAN_POINT('Ctrl Pts',(-3.33104452665746,0.936662886397859,-0.404003602504256));
#9579=CARTESIAN_POINT('Ctrl Pts',(-3.3522613707763,0.734173097051179,-0.708199221508163));
#9580=CARTESIAN_POINT('Ctrl Pts',(-3.37347821489514,0.450238919657464,-0.857314029843099));
#9581=CARTESIAN_POINT('Ctrl Pts',(-3.39469505901397,0.166304742263749,-1.00642883817804));
#9582=CARTESIAN_POINT('Ctrl Pts',(-3.41591190313281,-0.199073823176999,
-1.000462835844));
#9583=CARTESIAN_POINT('Ctrl Pts',(-3.43712874725165,-0.477988362584259,
-0.84215767843652));
#9584=CARTESIAN_POINT('Ctrl Pts',(-3.45834559137049,-0.756902901991522,
-0.683852521029037));
#9585=CARTESIAN_POINT('Ctrl Pts',(-3.47956243548932,-0.949353415365296,
-0.373208208548104));
#9586=CARTESIAN_POINT('Ctrl Pts',(-3.50077927960816,-0.966899956783025,
-0.0529802237674934));
#9587=CARTESIAN_POINT('Ctrl Pts',(-3.50194088077555,-0.967860612518642,
-0.0354480592821478));
#9588=CARTESIAN_POINT('Ctrl Pts',(-3.50310248194294,-0.968297001666331,
-0.0178871681811618));
#9589=CARTESIAN_POINT('Ctrl Pts',(-3.50426408311032,-0.968220991348266,
-0.000322423235073616));
#9590=CARTESIAN_POINT('Ctrl Pts',(-3.56223591688968,-0.968306026645575,
-0.000188088405189823));
#9591=CARTESIAN_POINT('Ctrl Pts',(-3.56157039554971,-0.968332773194304,
-0.0102491746403908));
#9592=CARTESIAN_POINT('Ctrl Pts',(-3.56090487420973,-0.968189594358999,
-0.0203094808260501));
#9593=CARTESIAN_POINT('Ctrl Pts',(-3.56023935286976,-0.967874149580525,
-0.0303643826376713));
#9594=CARTESIAN_POINT('Ctrl Pts',(-3.53902250875092,-0.957817758761798,
-0.35091501197702));
#9595=CARTESIAN_POINT('Ctrl Pts',(-3.51780566463208,-0.772681171152584,
-0.665972977747893));
#9596=CARTESIAN_POINT('Ctrl Pts',(-3.49658882051324,-0.49754324635805,-0.8307545242947));
#9597=CARTESIAN_POINT('Ctrl Pts',(-3.47537197639441,-0.222405321563516,
-0.995536070841506));
#9598=CARTESIAN_POINT('Ctrl Pts',(-3.45415513227557,0.142733940416339,-1.01004119816424));
#9599=CARTESIAN_POINT('Ctrl Pts',(-3.43293828815673,0.430076097675819,-0.867604123277958));
#9600=CARTESIAN_POINT('Ctrl Pts',(-3.4117214440379,0.717418254935302,-0.725167048391672));
#9601=CARTESIAN_POINT('Ctrl Pts',(-3.39050459991906,0.92696330747441,-0.425787771296361));
#9602=CARTESIAN_POINT('Ctrl Pts',(-3.36928775580022,0.962415574509713,-0.107044970905986));
#9603=CARTESIAN_POINT('Ctrl Pts',(-3.34807091168138,0.997867841545015,0.211697829484389));
#9604=CARTESIAN_POINT('Ctrl Pts',(-3.32685406756255,0.859227323076511,0.549804153169829));
#9605=CARTESIAN_POINT('Ctrl Pts',(-3.30563722344371,0.610205774310445,0.751898448216443));
#9606=CARTESIAN_POINT('Ctrl Pts',(-3.28442037932487,0.361184225544377,0.953992743263058));
#9607=CARTESIAN_POINT('Ctrl Pts',(-3.26320353520604,0.0017816464807463,
1.02007500967085));
#9608=CARTESIAN_POINT('Ctrl Pts',(-3.2419866910872,-0.302839792074258,0.919777377518324));
#9609=CARTESIAN_POINT('Ctrl Pts',(-3.22076984696836,-0.607461230629259,
0.8194797453658));
#9610=CARTESIAN_POINT('Ctrl Pts',(-3.19955300284952,-0.857301528675635,
0.552802214652963));
#9611=CARTESIAN_POINT('Ctrl Pts',(-3.17833615873069,-0.937547469887042,
0.242295491995441));
#9612=CARTESIAN_POINT('Ctrl Pts',(-3.17296941145035,-0.957845478598523,
0.163753598582142));
#9613=CARTESIAN_POINT('Ctrl Pts',(-3.16760266417001,-0.967292428537067,
0.082407407038659));
#9614=CARTESIAN_POINT('Ctrl Pts',(-3.16223591688968,-0.966552838587621,
0.000892251240061178));
#9615=CARTESIAN_POINT('Origin',(-2.4,0.,0.));
#9616=CARTESIAN_POINT('',(-2.70426408311032,-0.965152092930858,-7.43233170898139E-5));
#9617=CARTESIAN_POINT('',(-2.76223591688968,-0.965183717569061,-0.000198133119797293));
#9618=CARTESIAN_POINT('',(-2.4,-0.96675,-1.1839272930757E-16));
#9619=CARTESIAN_POINT('Ctrl Pts',(-2.70426408311032,-0.965152092930858,
-7.43233170898139E-5));
#9620=CARTESIAN_POINT('Ctrl Pts',(-2.71516701918355,-0.965038586003491,
0.166135545520124));
#9621=CARTESIAN_POINT('Ctrl Pts',(-2.72606995525678,-0.92432425151862,0.332397527830306));
#9622=CARTESIAN_POINT('Ctrl Pts',(-2.73697289133001,-0.84332535477354,0.475925179418795));
#9623=CARTESIAN_POINT('Ctrl Pts',(-2.75818973544885,-0.685703503696419,
0.755226441944987));
#9624=CARTESIAN_POINT('Ctrl Pts',(-2.77940657956769,-0.375531274417611,
0.948436890641441));
#9625=CARTESIAN_POINT('Ctrl Pts',(-2.80062342368653,-0.0553472065884891,
0.9667673541924));
#9626=CARTESIAN_POINT('Ctrl Pts',(-2.82184026780537,0.264836861240633,0.985097817743359));
#9627=CARTESIAN_POINT('Ctrl Pts',(-2.8430571119242,0.595032767620072,0.828548296148823));
#9628=CARTESIAN_POINT('Ctrl Pts',(-2.86427395604304,0.78350016363631,0.569060562673251));
#9629=CARTESIAN_POINT('Ctrl Pts',(-2.88549080016188,0.971967559652549,0.309572829197681));
#9630=CARTESIAN_POINT('Ctrl Pts',(-2.90670764428072,1.01870644530559,-0.0528531161589226));
#9631=CARTESIAN_POINT('Ctrl Pts',(-2.92792448839955,0.902238132701403,-0.351665725239072));
#9632=CARTESIAN_POINT('Ctrl Pts',(-2.94914133251839,0.785769820097216,-0.650478334319222));
#9633=CARTESIAN_POINT('Ctrl Pts',(-2.97035817663723,0.5060943092358,-0.885677607122917));
#9634=CARTESIAN_POINT('Ctrl Pts',(-2.99157502075606,0.191735481792182,-0.949178558246042));
#9635=CARTESIAN_POINT('Ctrl Pts',(-3.0127918648749,-0.122623345651437,-1.01267950936917));
#9636=CARTESIAN_POINT('Ctrl Pts',(-3.03400870899374,-0.471665489677259,
-0.904482138811726));
#9637=CARTESIAN_POINT('Ctrl Pts',(-3.05522555311258,-0.694989880204776,
-0.674308161611878));
#9638=CARTESIAN_POINT('Ctrl Pts',(-3.07157172977849,-0.867046568792577,
-0.496974319022883));
#9639=CARTESIAN_POINT('Ctrl Pts',(-3.08791790644441,-0.964481165861626,
-0.247239011638869));
#9640=CARTESIAN_POINT('Ctrl Pts',(-3.10426408311032,-0.966781343451459,
0.000892257579201902));
#9641=CARTESIAN_POINT('Ctrl Pts',(-3.16223591688968,-0.966552838587621,
0.000892251240061178));
#9642=CARTESIAN_POINT('Ctrl Pts',(-3.14638582005118,-0.964368541152476,
-0.23985378089515));
#9643=CARTESIAN_POINT('Ctrl Pts',(-3.13053572321268,-0.873332032515437,
-0.482073605686756));
#9644=CARTESIAN_POINT('Ctrl Pts',(-3.11468562637417,-0.710561968203914,
-0.657878448520745));
#9645=CARTESIAN_POINT('Ctrl Pts',(-3.09346878225534,-0.492678940932944,
-0.893209751777191));
#9646=CARTESIAN_POINT('Ctrl Pts',(-3.0722519381365,-0.14626130201457,-1.00953644368787));
#9647=CARTESIAN_POINT('Ctrl Pts',(-3.05103509401766,0.169495960438999,-0.953401008570004));
#9648=CARTESIAN_POINT('Ctrl Pts',(-3.02981824989883,0.48525322289257,-0.897265573452136));
#9649=CARTESIAN_POINT('Ctrl Pts',(-3.00860140577999,0.770350108881336,-0.668668011305719));
#9650=CARTESIAN_POINT('Ctrl Pts',(-2.98738456166115,0.893771363149558,-0.372659515025731));
#9651=CARTESIAN_POINT('Ctrl Pts',(-2.96616771754231,1.01719261741778,-0.0766510187457489));
#9652=CARTESIAN_POINT('Ctrl Pts',(-2.94495087342347,0.978938239965464,0.286768411667798));
#9653=CARTESIAN_POINT('Ctrl Pts',(-2.92373402930464,0.796587893266717,0.550590675567396));
#9654=CARTESIAN_POINT('Ctrl Pts',(-2.9025171851858,0.614237546567969,0.814412939466997));
#9655=CARTESIAN_POINT('Ctrl Pts',(-2.88130034106696,0.287791230622784,0.978638036852644));
#9656=CARTESIAN_POINT('Ctrl Pts',(-2.86008349694813,-0.0327338165447979,
0.967796911022139));
#9657=CARTESIAN_POINT('Ctrl Pts',(-2.83886665282929,-0.353258863712379,
0.956955785191634));
#9658=CARTESIAN_POINT('Ctrl Pts',(-2.81764980871045,-0.667862642102358,
0.771048436144978));
#9659=CARTESIAN_POINT('Ctrl Pts',(-2.79643296459161,-0.831970109502369,
0.495507921854437));
#9660=CARTESIAN_POINT('Ctrl Pts',(-2.78503394869097,-0.920138906889463,
0.347470320876771));
#9661=CARTESIAN_POINT('Ctrl Pts',(-2.77363493279032,-0.964866785481024,
0.173560012275024));
#9662=CARTESIAN_POINT('Ctrl Pts',(-2.76223591688968,-0.965183717569061,
-0.000198133119797293));
#9663=CARTESIAN_POINT('Origin',(-2.4,0.,0.));
#9664=CARTESIAN_POINT('',(-2.30426408311032,-0.967055040334201,-0.000867435447666626));
#9665=CARTESIAN_POINT('',(-2.36223591688968,-0.967282218044079,-0.000825613451897639));
#9666=CARTESIAN_POINT('',(-2.4,-0.96675,-1.1839272930757E-16));
#9667=CARTESIAN_POINT('Ctrl Pts',(-2.30426408311032,-0.967055040334201,
-0.000867435447666626));
#9668=CARTESIAN_POINT('Ctrl Pts',(-2.32119928780386,-0.964672432689995,
0.256018648921427));
#9669=CARTESIAN_POINT('Ctrl Pts',(-2.3381344924974,-0.859294642069947,0.514631033886055));
#9670=CARTESIAN_POINT('Ctrl Pts',(-2.35506969719094,-0.676007598850366,
0.693336971973552));
#9671=CARTESIAN_POINT('Ctrl Pts',(-2.37628654130978,-0.446381048987894,
0.917224199800165));
#9672=CARTESIAN_POINT('Ctrl Pts',(-2.39750338542862,-0.0944704787433332,
1.01569267115623));
#9673=CARTESIAN_POINT('Ctrl Pts',(-2.41872022954746,0.21800486678149,0.943491551879717));
#9674=CARTESIAN_POINT('Ctrl Pts',(-2.43993707366629,0.530480212306315,0.871290432603207));
#9675=CARTESIAN_POINT('Ctrl Pts',(-2.46115391778513,0.803520333111403,0.628419722694123));
#9676=CARTESIAN_POINT('Ctrl Pts',(-2.48237076190397,0.911650617313467,0.326489789060507));
#9677=CARTESIAN_POINT('Ctrl Pts',(-2.50358760602281,1.01978090151553,0.0245598554268904));
#9678=CARTESIAN_POINT('Ctrl Pts',(-2.52480445014164,0.963001349114571,-0.336429301931258));
#9679=CARTESIAN_POINT('Ctrl Pts',(-2.54602129426048,0.767404800530533,-0.590586405644005));
#9680=CARTESIAN_POINT('Ctrl Pts',(-2.56723813837932,0.571808251946495,-0.844743509356751));
#9681=CARTESIAN_POINT('Ctrl Pts',(-2.58845498249815,0.237394707179379,-0.992068559424097));
#9682=CARTESIAN_POINT('Ctrl Pts',(-2.60967182661699,-0.0821572842064791,
-0.964858855512405));
#9683=CARTESIAN_POINT('Ctrl Pts',(-2.63088867073583,-0.401709275592335,
-0.937649151600713));
#9684=CARTESIAN_POINT('Ctrl Pts',(-2.65210551485467,-0.706399713596932,
-0.735904693709986));
#9685=CARTESIAN_POINT('Ctrl Pts',(-2.67332235897351,-0.856209196161513,
-0.452336426586659));
#9686=CARTESIAN_POINT('Ctrl Pts',(-2.68363626701911,-0.929034410829473,
-0.314488544244662));
#9687=CARTESIAN_POINT('Ctrl Pts',(-2.69395017506472,-0.965259467678682,
-0.157304751152784));
#9688=CARTESIAN_POINT('Ctrl Pts',(-2.70426408311032,-0.965152092930858,
-7.43233170898139E-5));
#9689=CARTESIAN_POINT('Ctrl Pts',(-2.76223591688968,-0.965183717569061,
-0.000198133119797293));
#9690=CARTESIAN_POINT('Ctrl Pts',(-2.75241808867149,-0.965456687167867,
-0.149853826020577));
#9691=CARTESIAN_POINT('Ctrl Pts',(-2.7426002604533,-0.932784910411027,-0.299396641834704));
#9692=CARTESIAN_POINT('Ctrl Pts',(-2.7327824322351,-0.86654862044099,-0.432198857168075));
#9693=CARTESIAN_POINT('Ctrl Pts',(-2.71156558811627,-0.723408507569556,
-0.719191442365618));
#9694=CARTESIAN_POINT('Ctrl Pts',(-2.69034874399743,-0.423517125416644,
-0.92800293322628));
#9695=CARTESIAN_POINT('Ctrl Pts',(-2.66913189987859,-0.10468848707195,-0.962674755252969));
#9696=CARTESIAN_POINT('Ctrl Pts',(-2.64791505575975,0.214140151272745,-0.997346577279658));
#9697=CARTESIAN_POINT('Ctrl Pts',(-2.62669821164091,0.551906045809226,-0.857878730472374));
#9698=CARTESIAN_POINT('Ctrl Pts',(-2.60548136752208,0.753390086615068,-0.608363165482855));
#9699=CARTESIAN_POINT('Ctrl Pts',(-2.58426452340324,0.954874127420909,-0.358847600493338));
#9700=CARTESIAN_POINT('Ctrl Pts',(-2.56304767928441,1.02007631449612,0.000715682678407888));
#9701=CARTESIAN_POINT('Ctrl Pts',(-2.54183083516557,0.919033215752248,0.305090662050262));
#9702=CARTESIAN_POINT('Ctrl Pts',(-2.52061399104673,0.817990117008378,0.609465641422118));
#9703=CARTESIAN_POINT('Ctrl Pts',(-2.49939714692789,0.550701732445421,0.858652316994081));
#9704=CARTESIAN_POINT('Ctrl Pts',(-2.47818030280905,0.239999484108795,0.938137842405824));
#9705=CARTESIAN_POINT('Ctrl Pts',(-2.45696345869021,-0.0707027642278306,
1.01762336781757));
#9706=CARTESIAN_POINT('Ctrl Pts',(-2.43574661457138,-0.424818876338124,
0.927407743069098));
#9707=CARTESIAN_POINT('Ctrl Pts',(-2.41452977045254,-0.659616058236806,
0.708949236153339));
#9708=CARTESIAN_POINT('Ctrl Pts',(-2.39709848593159,-0.852520170623642,
0.529468613646879));
#9709=CARTESIAN_POINT('Ctrl Pts',(-2.37966720141063,-0.964885221791409,
0.263425353347209));
#9710=CARTESIAN_POINT('Ctrl Pts',(-2.36223591688968,-0.967282218044079,
-0.000825613451897639));
#9711=CARTESIAN_POINT('Origin',(-2.4,0.,0.));
#9712=CARTESIAN_POINT('',(-1.90426408311032,-0.968071505635494,0.000470124629695142));
#9713=CARTESIAN_POINT('',(-1.96223591688968,-0.967911638173995,0.000581251200357306));
#9714=CARTESIAN_POINT('',(-2.4,-0.96675,-1.1839272930757E-16));
#9715=CARTESIAN_POINT('Ctrl Pts',(-1.90426408311032,-0.968071505635494,
0.000470124629695142));
#9716=CARTESIAN_POINT('Ctrl Pts',(-1.90601471230534,-0.96822970479395,0.0269524939114589));
#9717=CARTESIAN_POINT('Ctrl Pts',(-1.90776534150035,-0.967237650430015,
0.0534228283859359));
#9718=CARTESIAN_POINT('Ctrl Pts',(-1.90951597069536,-0.96505709957596,0.0797948930788978));
#9719=CARTESIAN_POINT('Ctrl Pts',(-1.9307328148142,-0.938629796926441,0.399412540994581));
#9720=CARTESIAN_POINT('Ctrl Pts',(-1.95194965893303,-0.737631879641197,
0.704595971981054));
#9721=CARTESIAN_POINT('Ctrl Pts',(-1.97316650305187,-0.454431222389883,
0.855099230808537));
#9722=CARTESIAN_POINT('Ctrl Pts',(-1.99438334717071,-0.171230565138569,
1.00560248963602));
#9723=CARTESIAN_POINT('Ctrl Pts',(-2.01560019128955,0.19417283207881,1.00142557630451));
#9724=CARTESIAN_POINT('Ctrl Pts',(-2.03681703540838,0.473859143733365,0.844487976414537));
#9725=CARTESIAN_POINT('Ctrl Pts',(-2.05803387952722,0.75354545538792,0.687550376524566));
#9726=CARTESIAN_POINT('Ctrl Pts',(-2.07925072364606,0.947514681479651,0.377852090076135));
#9727=CARTESIAN_POINT('Ctrl Pts',(-2.1004675677649,0.966628957255425,0.0577138579841232));
#9728=CARTESIAN_POINT('Ctrl Pts',(-2.12168441188373,0.9857432330312,-0.262424374107885));
#9729=CARTESIAN_POINT('Ctrl Pts',(-2.14290125600257,0.830002558491023,-0.593002551843474));
#9730=CARTESIAN_POINT('Ctrl Pts',(-2.16411810012141,0.570977004122725,-0.782104654871943));
#9731=CARTESIAN_POINT('Ctrl Pts',(-2.18533494424024,0.311951449754423,-0.971206757900415));
#9732=CARTESIAN_POINT('Ctrl Pts',(-2.20655178835908,-0.0503589844420049,
-1.01883278622176));
#9733=CARTESIAN_POINT('Ctrl Pts',(-2.22776863247792,-0.349455833046081,
-0.903096368699818));
#9734=CARTESIAN_POINT('Ctrl Pts',(-2.24898547659676,-0.648552681650159,
-0.787359951177873));
#9735=CARTESIAN_POINT('Ctrl Pts',(-2.27020232071559,-0.884435944661884,
-0.508261087812633));
#9736=CARTESIAN_POINT('Ctrl Pts',(-2.29141916483443,-0.948706311427554,
-0.194058663981429));
#9737=CARTESIAN_POINT('Ctrl Pts',(-2.29570080425973,-0.961676314632596,
-0.130651425946197));
#9738=CARTESIAN_POINT('Ctrl Pts',(-2.29998244368503,-0.967657422591106,
-0.0658146035834261));
#9739=CARTESIAN_POINT('Ctrl Pts',(-2.30426408311032,-0.967055040334201,
-0.000867435447666626));
#9740=CARTESIAN_POINT('Ctrl Pts',(-2.36223591688968,-0.967282218044079,
-0.000825613451897639));
#9741=CARTESIAN_POINT('Ctrl Pts',(-2.3584503572918,-0.967802774756894,-0.058213110191665));
#9742=CARTESIAN_POINT('Ctrl Pts',(-2.35466479769391,-0.963136908454443,
-0.115516076998911));
#9743=CARTESIAN_POINT('Ctrl Pts',(-2.35087923809603,-0.952983195364544,
-0.171829546583339));
#9744=CARTESIAN_POINT('Ctrl Pts',(-2.32966239397719,-0.896074898906534,
-0.487448433321209));
#9745=CARTESIAN_POINT('Ctrl Pts',(-2.30844554985835,-0.666780054303452,
-0.771984817713898));
#9746=CARTESIAN_POINT('Ctrl Pts',(-2.28722870573952,-0.370470288071481,
-0.89468102102509));
#9747=CARTESIAN_POINT('Ctrl Pts',(-2.26601186162068,-0.0741605218395108,
-1.01737722433628));
#9748=CARTESIAN_POINT('Ctrl Pts',(-2.24479501750184,0.289164166021346,-0.978233246565974));
#9749=CARTESIAN_POINT('Ctrl Pts',(-2.22357817338301,0.552539213443868,-0.795237562828352));
#9750=CARTESIAN_POINT('Ctrl Pts',(-2.20236132926417,0.815914260866387,-0.612241879090731));
#9751=CARTESIAN_POINT('Ctrl Pts',(-2.18114448514533,0.979339667850574,-0.285394489385793));
#9752=CARTESIAN_POINT('Ctrl Pts',(-2.15992764102649,0.967713872572066,0.0351030562452503));
#9753=CARTESIAN_POINT('Ctrl Pts',(-2.13871079690766,0.956088077293558,0.355600601876296));
#9754=CARTESIAN_POINT('Ctrl Pts',(-2.11749395278882,0.769411079752361,0.669748303433444));
#9755=CARTESIAN_POINT('Ctrl Pts',(-2.09627710866998,0.493469627130093,0.833180707185582));
#9756=CARTESIAN_POINT('Ctrl Pts',(-2.07506026455115,0.217528174507824,0.99661311093772));
#9757=CARTESIAN_POINT('Ctrl Pts',(-2.05384342043231,-0.147677733195521,
1.00933021688484));
#9758=CARTESIAN_POINT('Ctrl Pts',(-2.03262657631347,-0.434319026055618,
0.865487924429265));
#9759=CARTESIAN_POINT('Ctrl Pts',(-2.01140973219463,-0.720960318915714,
0.721645631973692));
#9760=CARTESIAN_POINT('Ctrl Pts',(-1.99019288807579,-0.92903699693257,0.421243941115431));
#9761=CARTESIAN_POINT('Ctrl Pts',(-1.96897604395696,-0.962928166228546,
0.102331375488163));
#9762=CARTESIAN_POINT('Ctrl Pts',(-1.96672933493453,-0.966516993832283,
0.0685608611483841));
#9763=CARTESIAN_POINT('Ctrl Pts',(-1.9644826259121,-0.968152633160033,0.0345827794636375));
#9764=CARTESIAN_POINT('Ctrl Pts',(-1.96223591688968,-0.967911638173995,
0.000581251200357305));
#9765=CARTESIAN_POINT('Origin',(-2.4,0.,0.));
#9766=CARTESIAN_POINT('',(-1.50426408311032,-0.965599742549273,0.000642173102301594));
#9767=CARTESIAN_POINT('',(-1.56223591688968,-0.965458677004063,0.000548056880589385));
#9768=CARTESIAN_POINT('',(-2.4,-0.96675,-1.1839272930757E-16));
#9769=CARTESIAN_POINT('Ctrl Pts',(-1.50426408311032,-0.965599742549273,
0.000642173102301594));
#9770=CARTESIAN_POINT('Ctrl Pts',(-1.51204698092564,-0.966318997139783,
0.11915113060191));
#9771=CARTESIAN_POINT('Ctrl Pts',(-1.51982987874097,-0.946135628360824,
0.237423627428648));
#9772=CARTESIAN_POINT('Ctrl Pts',(-1.52761277655629,-0.903949191798766,
0.347243846254945));
#9773=CARTESIAN_POINT('Ctrl Pts',(-1.54882962067513,-0.788945362928715,
0.646623141630892));
#9774=CARTESIAN_POINT('Ctrl Pts',(-1.57004646479396,-0.510424820094816,
0.883188981275794));
#9775=CARTESIAN_POINT('Ctrl Pts',(-1.5912633089128,-0.196380683128556,0.948228378521808));
#9776=CARTESIAN_POINT('Ctrl Pts',(-1.61248015303164,0.117663453837714,1.01326777576782));
#9777=CARTESIAN_POINT('Ctrl Pts',(-1.63369699715047,0.46723118493635,0.90678073061494));
#9778=CARTESIAN_POINT('Ctrl Pts',(-1.65491384126931,0.691679908206297,0.677702984351692));
#9779=CARTESIAN_POINT('Ctrl Pts',(-1.67613068538815,0.91612863147624,0.448625238088448));
#9780=CARTESIAN_POINT('Ctrl Pts',(-1.69734752950699,1.0154583469175,0.0969567907148498));
#9781=CARTESIAN_POINT('Ctrl Pts',(-1.71856437362582,0.944022438840599,-0.21569437946784));
#9782=CARTESIAN_POINT('Ctrl Pts',(-1.73978121774466,0.872586530763696,-0.528345549650531));
#9783=CARTESIAN_POINT('Ctrl Pts',(-1.7609980618635,0.630384999168622,-0.80197944264231));
#9784=CARTESIAN_POINT('Ctrl Pts',(-1.78221490598234,0.328720692399986,-0.91084858062028));
#9785=CARTESIAN_POINT('Ctrl Pts',(-1.80343175010117,0.027056385631351,-1.01971771859825));
#9786=CARTESIAN_POINT('Ctrl Pts',(-1.82464859422001,-0.334070696310848,
-0.96382210156241));
#9787=CARTESIAN_POINT('Ctrl Pts',(-1.84586543833885,-0.588705893275055,
-0.768848360622047));
#9788=CARTESIAN_POINT('Ctrl Pts',(-1.86533165326267,-0.822330811453852,
-0.589962154719374));
#9789=CARTESIAN_POINT('Ctrl Pts',(-1.8847978681865,-0.966312401635604,-0.29400199636517));
#9790=CARTESIAN_POINT('Ctrl Pts',(-1.90426408311032,-0.968071505635494,
0.000470124629695142));
#9791=CARTESIAN_POINT('Ctrl Pts',(-1.96223591688968,-0.967911638173995,
0.000581251200357305));
#9792=CARTESIAN_POINT('Ctrl Pts',(-1.94326578179327,-0.965876791917949,
-0.28651137103078));
#9793=CARTESIAN_POINT('Ctrl Pts',(-1.92429564669686,-0.830050963541899,
-0.575275571334595));
#9794=CARTESIAN_POINT('Ctrl Pts',(-1.90532551160045,-0.606516910331822,
-0.75487720935754));
#9795=CARTESIAN_POINT('Ctrl Pts',(-1.88410866748161,-0.356508824564027,
-0.955749788179695));
#9796=CARTESIAN_POINT('Ctrl Pts',(-1.86289182336277,0.00321300754665053,
-1.02007150542773));
#9797=CARTESIAN_POINT('Ctrl Pts',(-1.84167497924393,0.307339703415352,-0.91828354577121));
#9798=CARTESIAN_POINT('Ctrl Pts',(-1.8204581351251,0.611466399284058,-0.816495586114686));
#9799=CARTESIAN_POINT('Ctrl Pts',(-1.79924129100626,0.859997958910781,-0.548597949553592));
#9800=CARTESIAN_POINT('Ctrl Pts',(-1.77802444688742,0.938722592134658,-0.2377020377213));
#9801=CARTESIAN_POINT('Ctrl Pts',(-1.75680760276859,1.01744722535853,0.0731938741109885));
#9802=CARTESIAN_POINT('Ctrl Pts',(-1.73559075864975,0.926364932179567,0.427088061214477));
#9803=CARTESIAN_POINT('Ctrl Pts',(-1.71437391453091,0.707332254956844,0.661349714465122));
#9804=CARTESIAN_POINT('Ctrl Pts',(-1.69315707041207,0.48829957773412,0.895611367715769));
#9805=CARTESIAN_POINT('Ctrl Pts',(-1.67194022629324,0.141316516467642,1.01024048711357));
#9806=CARTESIAN_POINT('Ctrl Pts',(-1.6507233821744,-0.174162102857795,0.952559670401592));
#9807=CARTESIAN_POINT('Ctrl Pts',(-1.62950653805556,-0.489640722183227,
0.894878853689613));
#9808=CARTESIAN_POINT('Ctrl Pts',(-1.60828969393672,-0.773614899567618,
0.664888100867853));
#9809=CARTESIAN_POINT('Ctrl Pts',(-1.58707284981789,-0.895585316547392,
0.368278840650108));
#9810=CARTESIAN_POINT('Ctrl Pts',(-1.57879387217515,-0.943179122185725,
0.252539599685851));
#9811=CARTESIAN_POINT('Ctrl Pts',(-1.57051489453241,-0.966105893179072,
0.126656884114399));
#9812=CARTESIAN_POINT('Ctrl Pts',(-1.56223591688968,-0.965458677004063,
0.000548056880589385));
#9813=CARTESIAN_POINT('Origin',(-2.4,0.,0.));
#9814=CARTESIAN_POINT('',(-1.10426408311032,-0.965723377661902,-0.000706068753700967));
#9815=CARTESIAN_POINT('',(-1.16223591688968,-0.965902006734961,-0.000776836658390276));
#9816=CARTESIAN_POINT('',(-2.4,-0.96675,-1.1839272930757E-16));
#9817=CARTESIAN_POINT('Ctrl Pts',(-1.10426408311032,-0.965723377661902,
-0.000706068753700967));
#9818=CARTESIAN_POINT('Ctrl Pts',(-1.11807924954595,-0.964308267852233,
0.209587692729153));
#9819=CARTESIAN_POINT('Ctrl Pts',(-1.13189441598158,-0.896836495797635,
0.420708008852773));
#9820=CARTESIAN_POINT('Ctrl Pts',(-1.14570958241722,-0.770287306902609,
0.586821847481257));
#9821=CARTESIAN_POINT('Ctrl Pts',(-1.16692642653605,-0.575937537273619,
0.841933607197183));
#9822=CARTESIAN_POINT('Ctrl Pts',(-1.18814327065489,-0.242249365485617,
0.990894302828568));
#9823=CARTESIAN_POINT('Ctrl Pts',(-1.20936011477373,0.0774320207124568,
0.965249562113937));
#9824=CARTESIAN_POINT('Ctrl Pts',(-1.23057695889257,0.397113406910531,0.939604821399306));
#9825=CARTESIAN_POINT('Ctrl Pts',(-1.2517938030114,0.70278800751868,0.73935464433866));
#9826=CARTESIAN_POINT('Ctrl Pts',(-1.27301064713024,0.853984141923179,0.456523293143792));
#9827=CARTESIAN_POINT('Ctrl Pts',(-1.29422749124908,1.00518027632768,0.173691941948927));
#9828=CARTESIAN_POINT('Ctrl Pts',(-1.31544433536791,1.00189794452853,-0.191720583380155));
#9829=CARTESIAN_POINT('Ctrl Pts',(-1.33666117948675,0.84564553572297,-0.471790267208678));
#9830=CARTESIAN_POINT('Ctrl Pts',(-1.35787802360559,0.689393126917406,-0.751859951037208));
#9831=CARTESIAN_POINT('Ctrl Pts',(-1.37909486772443,0.380170641105417,-0.94658679336517));
#9832=CARTESIAN_POINT('Ctrl Pts',(-1.40031171184326,0.0600801639036459,
-0.966484767136129));
#9833=CARTESIAN_POINT('Ctrl Pts',(-1.4215285559621,-0.26001031329812,-0.986382740907086));
#9834=CARTESIAN_POINT('Ctrl Pts',(-1.44274540008094,-0.59096878188967,-0.831451846121045));
#9835=CARTESIAN_POINT('Ctrl Pts',(-1.46396224419978,-0.780704458732344,
-0.572890023174525));
#9836=CARTESIAN_POINT('Ctrl Pts',(-1.47739619050329,-0.900840086834668,
-0.409175493994447));
#9837=CARTESIAN_POINT('Ctrl Pts',(-1.49083013680681,-0.964358247700343,
-0.203914408432289));
#9838=CARTESIAN_POINT('Ctrl Pts',(-1.50426408311032,-0.965599742549273,
0.000642173102301594));
#9839=CARTESIAN_POINT('Ctrl Pts',(-1.56223591688968,-0.965458677004063,
0.000548056880589385));
#9840=CARTESIAN_POINT('Ctrl Pts',(-1.54929805041358,-0.964447248200316,
-0.19652690075507));
#9841=CARTESIAN_POINT('Ctrl Pts',(-1.53636018393748,-0.905864663033144,
-0.394154056445996));
#9842=CARTESIAN_POINT('Ctrl Pts',(-1.52342231746137,-0.79388246609903,-0.554484439595403));
#9843=CARTESIAN_POINT('Ctrl Pts',(-1.50220547334254,-0.610242542095736,
-0.817410692009432));
#9844=CARTESIAN_POINT('Ctrl Pts',(-1.4809886292237,-0.282996037513986,-0.980035429223758));
#9845=CARTESIAN_POINT('Ctrl Pts',(-1.45977178510486,0.0374720856061225,
-0.967625034121375));
#9846=CARTESIAN_POINT('Ctrl Pts',(-1.43855494098602,0.357940208726231,-0.955214639018993));
#9847=CARTESIAN_POINT('Ctrl Pts',(-1.41733809686719,0.671629950384701,-0.767769111599907));
#9848=CARTESIAN_POINT('Ctrl Pts',(-1.39612125274835,0.834386311033359,-0.491428374630777));
#9849=CARTESIAN_POINT('Ctrl Pts',(-1.37490440862951,0.997142671682019,-0.215087637661645));
#9850=CARTESIAN_POINT('Ctrl Pts',(-1.35368756451068,1.00896565132086,0.150148308857529));
#9851=CARTESIAN_POINT('Ctrl Pts',(-1.33247072039184,0.864422041242199,0.436436591579802));
#9852=CARTESIAN_POINT('Ctrl Pts',(-1.311253876273,0.719878431163536,0.722724874302071));
#9853=CARTESIAN_POINT('Ctrl Pts',(-1.29003703215416,0.418968231367369,0.930065493227438));
#9854=CARTESIAN_POINT('Ctrl Pts',(-1.26882018803533,0.0999736502051578,
0.963175806270917));
#9855=CARTESIAN_POINT('Ctrl Pts',(-1.24760334391649,-0.219020930957061,
0.996286119314397));
#9856=CARTESIAN_POINT('Ctrl Pts',(-1.22638649979765,-0.556099893485328,
0.855166126475976));
#9857=CARTESIAN_POINT('Ctrl Pts',(-1.20516965567881,-0.756359806986027,
0.604667019117695));
#9858=CARTESIAN_POINT('Ctrl Pts',(-1.19085840941577,-0.891439695525161,
0.43569964611925));
#9859=CARTESIAN_POINT('Ctrl Pts',(-1.17654716315272,-0.964269505163745,
0.216966845299701));
#9860=CARTESIAN_POINT('Ctrl Pts',(-1.16223591688968,-0.965902006734961,
-0.000776836658390276));
#9861=CARTESIAN_POINT('Origin',(-2.4,0.,0.));
#9862=CARTESIAN_POINT('',(-0.70426408311032,-0.968174375420009,-0.000375732050173772));
#9863=CARTESIAN_POINT('',(-0.762235916889676,-0.96827543336235,-0.000245152029857915));
#9864=CARTESIAN_POINT('',(-2.4,-0.96675,-1.1839272930757E-16));
#9865=CARTESIAN_POINT('Ctrl Pts',(-0.70426408311032,-0.968174375420009,
-0.000375732050173772));
#9866=CARTESIAN_POINT('Ctrl Pts',(-0.724111518166262,-0.966689092810169,
0.299779414582345));
#9867=CARTESIAN_POINT('Ctrl Pts',(-0.743958953222203,-0.816237650885706,
0.601218448215989));
#9868=CARTESIAN_POINT('Ctrl Pts',(-0.763806388278144,-0.574799344401601,
0.779299351345548));
#9869=CARTESIAN_POINT('Ctrl Pts',(-0.785023232396981,-0.316702572775889,
0.969667262946833));
#9870=CARTESIAN_POINT('Ctrl Pts',(-0.806240076515818,0.0453698123326327,
1.01906716384315));
#9871=CARTESIAN_POINT('Ctrl Pts',(-0.827456920634656,0.345029639018638,
0.904796719287963));
#9872=CARTESIAN_POINT('Ctrl Pts',(-0.848673764753493,0.644689465704639,
0.79052627473278));
#9873=CARTESIAN_POINT('Ctrl Pts',(-0.86989060887233,0.881936733968123,0.512585484726105));
#9874=CARTESIAN_POINT('Ctrl Pts',(-0.891107452991167,0.947744835699073,
0.198701460812145));
#9875=CARTESIAN_POINT('Ctrl Pts',(-0.912324297110005,1.01355293743002,-0.115182563101821));
#9876=CARTESIAN_POINT('Ctrl Pts',(-0.933541141228843,0.907921872628429,
-0.465009820923077));
#9877=CARTESIAN_POINT('Ctrl Pts',(-0.95475798534768,0.679394269325379,-0.690018664841971));
#9878=CARTESIAN_POINT('Ctrl Pts',(-0.975974829466518,0.45086666602233,-0.915027508760864));
#9879=CARTESIAN_POINT('Ctrl Pts',(-0.997191673585356,0.0994425242178281,
-1.0152179387774));
#9880=CARTESIAN_POINT('Ctrl Pts',(-1.01840851770419,-0.213382578998573,
-0.944547685625948));
#9881=CARTESIAN_POINT('Ctrl Pts',(-1.03962536182303,-0.526207682214969,
-0.873877432474494));
#9882=CARTESIAN_POINT('Ctrl Pts',(-1.06084220594187,-0.800433746843263,
-0.632346496155052));
#9883=CARTESIAN_POINT('Ctrl Pts',(-1.0820590500607,-0.910041095422422,-0.330949616095098));
#9884=CARTESIAN_POINT('Ctrl Pts',(-1.08946072774391,-0.94827855719335,-0.225804734583378));
#9885=CARTESIAN_POINT('Ctrl Pts',(-1.09686240542712,-0.966481543460795,
-0.113374030340516));
#9886=CARTESIAN_POINT('Ctrl Pts',(-1.10426408311032,-0.965723377661902,
-0.000706068753700967));
#9887=CARTESIAN_POINT('Ctrl Pts',(-1.16223591688968,-0.965902006734961,
-0.000776836658390276));
#9888=CARTESIAN_POINT('Ctrl Pts',(-1.15533031903388,-0.966689736827963,
-0.105844576784186));
#9889=CARTESIAN_POINT('Ctrl Pts',(-1.14842472117809,-0.950900264858972,
-0.210682015741653));
#9890=CARTESIAN_POINT('Ctrl Pts',(-1.1415191233223,-0.917528373311847,-0.309586901090642));
#9891=CARTESIAN_POINT('Ctrl Pts',(-1.12030227920346,-0.814996161663834,
-0.613463492062563));
#9892=CARTESIAN_POINT('Ctrl Pts',(-1.09908543508463,-0.546490873894676,
-0.861338452128276));
#9893=CARTESIAN_POINT('Ctrl Pts',(-1.07786859096579,-0.235403164132973,
-0.939301718640285));
#9894=CARTESIAN_POINT('Ctrl Pts',(-1.05665174684695,0.0756845456287358,
-1.01726498515229));
#9895=CARTESIAN_POINT('Ctrl Pts',(-1.03543490272812,0.429354677382993,-0.925316558110594));
#9896=CARTESIAN_POINT('Ctrl Pts',(-1.01421805860928,0.66307940207031,-0.705711028458576));
#9897=CARTESIAN_POINT('Ctrl Pts',(-0.993001214490441,0.896804126757628,
-0.486105498806557));
#9898=CARTESIAN_POINT('Ctrl Pts',(-0.971784370371604,1.01058344437801,-0.138842866544224));
#9899=CARTESIAN_POINT('Ctrl Pts',(-0.950567526252767,0.95213044525232,0.176493604177211));
#9900=CARTESIAN_POINT('Ctrl Pts',(-0.92935068213393,0.893677446126634,0.491830074898643));
#9901=CARTESIAN_POINT('Ctrl Pts',(-0.908133838015092,0.662992130254884,
0.775240384079175));
#9902=CARTESIAN_POINT('Ctrl Pts',(-0.886916993896254,0.366085168741984,
0.89648426537136));
#9903=CARTESIAN_POINT('Ctrl Pts',(-0.865700149777417,0.0691782072290847,
1.01772814666354));
#9904=CARTESIAN_POINT('Ctrl Pts',(-0.84448330565858,-0.293950399924966,
0.976805600067383));
#9905=CARTESIAN_POINT('Ctrl Pts',(-0.823266461539743,-0.556426309807427,
0.792522571211873));
#9906=CARTESIAN_POINT('Ctrl Pts',(-0.802922946656388,-0.808098167757085,
0.615825013400089));
#9907=CARTESIAN_POINT('Ctrl Pts',(-0.782579431773032,-0.967232937816001,
0.307326103945468));
#9908=CARTESIAN_POINT('Ctrl Pts',(-0.762235916889676,-0.96827543336235,
-0.000245152029857915));
#9909=CARTESIAN_POINT('Origin',(-2.4,0.,0.));
#9910=CARTESIAN_POINT('',(-0.304264083110319,-0.966880390654327,0.000888722329053411));
#9911=CARTESIAN_POINT('',(-0.362235916889675,-0.966647958720147,0.000894507509818508));
#9912=CARTESIAN_POINT('',(-2.4,-0.96675,-1.1839272930757E-16));
#9913=CARTESIAN_POINT('Ctrl Pts',(-0.304264083110319,-0.966880390654327,
0.000888722329053411));
#9914=CARTESIAN_POINT('Ctrl Pts',(-0.308926942667733,-0.967547389216313,
0.0716595015038585));
#9915=CARTESIAN_POINT('Ctrl Pts',(-0.313589802225146,-0.960449129896506,
0.142298216778232));
#9916=CARTESIAN_POINT('Ctrl Pts',(-0.31825266178256,-0.945090658341382,
0.211090037483764));
#9917=CARTESIAN_POINT('Ctrl Pts',(-0.339469505901397,-0.875206868603263,
0.524105113016059));
#9918=CARTESIAN_POINT('Ctrl Pts',(-0.360686350020234,-0.634302604231348,
0.798881850747375));
#9919=CARTESIAN_POINT('Ctrl Pts',(-0.381903194139071,-0.333164225454192,
0.90921732537962));
#9920=CARTESIAN_POINT('Ctrl Pts',(-0.403120038257909,-0.0320258466770354,
1.01955280001186));
#9921=CARTESIAN_POINT('Ctrl Pts',(-0.424336882376745,0.329346646505356,
0.965447011545035));
#9922=CARTESIAN_POINT('Ctrl Pts',(-0.445553726495582,0.584927785612826,
0.771727344806177));
#9923=CARTESIAN_POINT('Ctrl Pts',(-0.46677057061442,0.8405089247203,0.578007678067315));
#9924=CARTESIAN_POINT('Ctrl Pts',(-0.487987414733257,0.990298709752847,
0.244674133056408));
#9925=CARTESIAN_POINT('Ctrl Pts',(-0.509204258852095,0.965439664309523,
-0.0750716926308972));
#9926=CARTESIAN_POINT('Ctrl Pts',(-0.530421102970933,0.9405806188662,-0.394817518318202));
#9927=CARTESIAN_POINT('Ctrl Pts',(-0.55163794708977,0.741072742947015,-0.70097562468191));
#9928=CARTESIAN_POINT('Ctrl Pts',(-0.572854791208608,0.458610822756454,
-0.85286234921427));
#9929=CARTESIAN_POINT('Ctrl Pts',(-0.594071635327445,0.176148902565893,
-1.00474907374663));
#9930=CARTESIAN_POINT('Ctrl Pts',(-0.615288479446282,-0.18926706189604,
-1.00236441644764));
#9931=CARTESIAN_POINT('Ctrl Pts',(-0.636505323565119,-0.469717611786197,
-0.846798862084744));
#9932=CARTESIAN_POINT('Ctrl Pts',(-0.657722167683956,-0.75016816167635,
-0.691233307721851));
#9933=CARTESIAN_POINT('Ctrl Pts',(-0.678939011802793,-0.945653296994726,
-0.382486856295058));
#9934=CARTESIAN_POINT('Ctrl Pts',(-0.70015585592163,-0.96633528558247,-0.0624456694285343));
#9935=CARTESIAN_POINT('Ctrl Pts',(-0.701525264984527,-0.967670173205349,
-0.0417890958429217));
#9936=CARTESIAN_POINT('Ctrl Pts',(-0.702894674047424,-0.968276855133944,
-0.0210854699540959));
#9937=CARTESIAN_POINT('Ctrl Pts',(-0.70426408311032,-0.968174375420009,
-0.000375732050173772));
#9938=CARTESIAN_POINT('Ctrl Pts',(-0.762235916889676,-0.96827543336235,
-0.000245152029857915));
#9939=CARTESIAN_POINT('Ctrl Pts',(-0.761362587654194,-0.968320186781005,
-0.013448916048874));
#9940=CARTESIAN_POINT('Ctrl Pts',(-0.760489258418712,-0.968073590440504,
-0.0266509704864536));
#9941=CARTESIAN_POINT('Ctrl Pts',(-0.75961592918323,-0.967530457975804,
-0.0398408145552752));
#9942=CARTESIAN_POINT('Ctrl Pts',(-0.738399085064393,-0.95433548365085,
-0.360277660352052));
#9943=CARTESIAN_POINT('Ctrl Pts',(-0.717182240945555,-0.766122322390069,
-0.673507840830754));
#9944=CARTESIAN_POINT('Ctrl Pts',(-0.695965396826718,-0.489384059384532,
-0.835587057776708));
#9945=CARTESIAN_POINT('Ctrl Pts',(-0.674748552707881,-0.212645796378994,
-0.997666274722664));
#9946=CARTESIAN_POINT('Ctrl Pts',(-0.653531708589043,0.152617568371304,
-1.00859452813588));
#9947=CARTESIAN_POINT('Ctrl Pts',(-0.632314864470206,0.43855131866906,-0.863350704134818));
#9948=CARTESIAN_POINT('Ctrl Pts',(-0.611098020351369,0.724485068966817,
-0.71810688013376));
#9949=CARTESIAN_POINT('Ctrl Pts',(-0.589881176232532,0.931089204812032,
-0.41669097871843));
#9950=CARTESIAN_POINT('Ctrl Pts',(-0.568664332113694,0.963418095823207,
-0.097615843577119));
#9951=CARTESIAN_POINT('Ctrl Pts',(-0.547447487994857,0.995746986834382,
0.221459291564192));
#9952=CARTESIAN_POINT('Ctrl Pts',(-0.526230643876019,0.853800633011516,
0.558193660431483));
#9953=CARTESIAN_POINT('Ctrl Pts',(-0.505013799757181,0.602812702394469,
0.757838853851704));
#9954=CARTESIAN_POINT('Ctrl Pts',(-0.483796955638344,0.351824771777427,
0.957484047271921));
#9955=CARTESIAN_POINT('Ctrl Pts',(-0.462580111519508,-0.0082047356337903,
1.02004006524507));
#9956=CARTESIAN_POINT('Ctrl Pts',(-0.441363267400671,-0.311830722736786,
0.91676583738276));
#9957=CARTESIAN_POINT('Ctrl Pts',(-0.420146423281833,-0.615456709839787,
0.813491609520446));
#9958=CARTESIAN_POINT('Ctrl Pts',(-0.398929579162996,-0.862679176634563,
0.544387135822666));
#9959=CARTESIAN_POINT('Ctrl Pts',(-0.377712735044158,-0.939878100228005,
0.233106416590011));
#9960=CARTESIAN_POINT('Ctrl Pts',(-0.372553795659331,-0.958649250412349,
0.157417574592957));
#9961=CARTESIAN_POINT('Ctrl Pts',(-0.367394856274503,-0.967368033465226,
0.0792351302608346));
#9962=CARTESIAN_POINT('Ctrl Pts',(-0.362235916889675,-0.966647958720147,
0.000894507509818508));
#9963=CARTESIAN_POINT('Origin',(-5.57277255930238,0.,0.));
#9964=CARTESIAN_POINT('',(-0.172772559302379,-0.739099672814633,0.000679354332688233));
#9965=CARTESIAN_POINT('',(-0.0937274406976069,-0.737618920515246,-0.00032948291856405));
#9966=CARTESIAN_POINT('',(-5.57277255930238,-0.739,-6.04325409642289E-14));
#9967=CARTESIAN_POINT('',(-4.9849202071072E-16,0.673666798061217,-0.306809933949289));
#9968=CARTESIAN_POINT('Ctrl Pts',(-0.172772559302379,-0.739099672814633,
0.000679354332688226));
#9969=CARTESIAN_POINT('Ctrl Pts',(-0.156218574740956,-0.73728956115382,
-0.191379549432806));
#9970=CARTESIAN_POINT('Ctrl Pts',(-0.118447746060696,-0.562456718061683,
-0.632498879064449));
#9971=CARTESIAN_POINT('Ctrl Pts',(-0.0608568929599041,0.163603744986237,
-0.849599325325673));
#9972=CARTESIAN_POINT('Ctrl Pts',(-0.0198200244205333,0.577662614586297,
-0.514890579234534));
#9973=CARTESIAN_POINT('Ctrl Pts',(-4.54822811357669E-16,0.673678098462135,
-0.306812656843393));
#9974=CARTESIAN_POINT('',(0.,-0.0726952737146206,-0.735415798837336));
#9975=CARTESIAN_POINT('Origin',(0.,0.,0.));
#9976=CARTESIAN_POINT('Ctrl Pts',(-0.0937274406976069,-0.737618920515246,
-0.000329482918564024));
#9977=CARTESIAN_POINT('Ctrl Pts',(-0.0837018045839084,-0.737704674247543,
-0.117242503813553));
#9978=CARTESIAN_POINT('Ctrl Pts',(-0.0524593243513723,-0.656307493993609,
-0.481183238878904));
#9979=CARTESIAN_POINT('Ctrl Pts',(-0.0212168441188374,-0.31778980334938,
-0.71118839721512));
#9980=CARTESIAN_POINT('Ctrl Pts',(0.,-0.0726952737146206,-0.735415798837336));
#9981=CARTESIAN_POINT('Origin',(-5.57277255930238,0.,0.));
#9982=CARTESIAN_POINT('',(-0.572772559302381,-0.740088816586901,-0.000287215914272227));
#9983=CARTESIAN_POINT('',(-0.493727440697609,-0.738921997925201,0.000683776622396153));
#9984=CARTESIAN_POINT('',(-5.57277255930238,-0.739,-6.04325409642289E-14));
#9985=CARTESIAN_POINT('Ctrl Pts',(-0.57277255930238,-0.740088816586901,
-0.00028721591427226));
#9986=CARTESIAN_POINT('Ctrl Pts',(-0.571403150239485,-0.740167153808103,
-0.0161180887469435));
#9987=CARTESIAN_POINT('Ctrl Pts',(-0.548816897057752,-0.73251819520185,
-0.277146429890355));
#9988=CARTESIAN_POINT('Ctrl Pts',(-0.505013799757182,-0.424009057645233,
-0.764401388167426));
#9989=CARTESIAN_POINT('Ctrl Pts',(-0.441363267400671,0.413981315473058,
-0.769870004905825));
#9990=CARTESIAN_POINT('Ctrl Pts',(-0.377712735044158,0.871502868007656,
-0.0677727493502481));
#9991=CARTESIAN_POINT('Ctrl Pts',(-0.314062202687646,0.527997356327125,
0.696644596694906));
#9992=CARTESIAN_POINT('Ctrl Pts',(-0.250411670331135,-0.300720323926695,
0.82072272757771));
#9993=CARTESIAN_POINT('Ctrl Pts',(-0.203315122536045,-0.709494106736934,
0.354473087690529));
#9994=CARTESIAN_POINT('Ctrl Pts',(-0.177435418859794,-0.739609537761425,
0.0547777311728134));
#9995=CARTESIAN_POINT('Ctrl Pts',(-0.172772559302379,-0.739099672814633,
0.000679354332688226));
#9996=CARTESIAN_POINT('Ctrl Pts',(-0.493727440697609,-0.738921997925201,
0.000683776622396153));
#9997=CARTESIAN_POINT('Ctrl Pts',(-0.4776695359636,-0.737208686587061,-0.185716146597215));
#9998=CARTESIAN_POINT('Ctrl Pts',(-0.440394787110755,-0.570963787203614,
-0.62112020546076));
#9999=CARTESIAN_POINT('Ctrl Pts',(-0.381903194139071,0.161393004974118,
-0.859052194921053));
#10000=CARTESIAN_POINT('Ctrl Pts',(-0.318252661782561,0.810114474683083,
-0.328550731088526));
#10001=CARTESIAN_POINT('Ctrl Pts',(-0.254602129426047,0.714063928013904,
0.504165699398937));
#10002=CARTESIAN_POINT('Ctrl Pts',(-0.190951597069536,-0.0378944583360208,
0.873038406069037));
#10003=CARTESIAN_POINT('Ctrl Pts',(-0.137326700826723,-0.64268646989993,
0.508551427110721));
#10004=CARTESIAN_POINT('Ctrl Pts',(-0.104918648702746,-0.737523197127276,
0.130175745927442));
#10005=CARTESIAN_POINT('Ctrl Pts',(-0.0937274406976069,-0.737618920515246,
-0.000329482918564024));
#10006=CARTESIAN_POINT('Origin',(-5.57277255930238,0.,0.));
#10007=CARTESIAN_POINT('',(-0.972772559302382,-0.738215232575273,-0.000539730860128765));
#10008=CARTESIAN_POINT('',(-0.893727440697611,-0.740166066981926,-0.000187398345083065));
#10009=CARTESIAN_POINT('',(-5.57277255930238,-0.739,-6.04325409642289E-14));
#10010=CARTESIAN_POINT('Ctrl Pts',(-0.972772559302383,-0.738215232575273,
-0.000539730860128814));
#10011=CARTESIAN_POINT('Ctrl Pts',(-0.965370881619177,-0.738794787295084,
-0.0866650203482554));
#10012=CARTESIAN_POINT('Ctrl Pts',(-0.936752359817135,-0.684993839343999,
-0.418966455849));
#10013=CARTESIAN_POINT('Ctrl Pts',(-0.886916993896255,-0.192618997048393,
-0.852636963577682));
#10014=CARTESIAN_POINT('Ctrl Pts',(-0.823266461539743,0.613284620619645,
-0.622875201646802));
#10015=CARTESIAN_POINT('Ctrl Pts',(-0.759615929183231,0.855523121436939,
0.179366360897505));
#10016=CARTESIAN_POINT('Ctrl Pts',(-0.695965396826718,0.311455685450219,
0.816754239299164));
#10017=CARTESIAN_POINT('Ctrl Pts',(-0.633684273533102,-0.501003048588561,
0.705905186472791));
#10018=CARTESIAN_POINT('Ctrl Pts',(-0.592619994358323,-0.738953441517176,
0.229156438972142));
#10019=CARTESIAN_POINT('Ctrl Pts',(-0.57277255930238,-0.740088816586901,
-0.00028721591427226));
#10020=CARTESIAN_POINT('Ctrl Pts',(-0.89372744069761,-0.740166066981926,
-0.000187398345083168));
#10021=CARTESIAN_POINT('Ctrl Pts',(-0.892854111462129,-0.740200277249715,
-0.0102805781847964));
#10022=CARTESIAN_POINT('Ctrl Pts',(-0.870763938107811,-0.735432257888453,
-0.265546536466872));
#10023=CARTESIAN_POINT('Ctrl Pts',(-0.827456920634656,-0.441763506671353,
-0.754279180499295));
#10024=CARTESIAN_POINT('Ctrl Pts',(-0.763806388278142,0.395876917069436,
-0.779340403997693));
#10025=CARTESIAN_POINT('Ctrl Pts',(-0.700155855921632,0.869671971808336,
-0.0881182126992239));
#10026=CARTESIAN_POINT('Ctrl Pts',(-0.636505323565118,0.544153413313058,
0.68409807463336));
#10027=CARTESIAN_POINT('Ctrl Pts',(-0.572854791208608,-0.281484464039597,
0.827554699248267));
#10028=CARTESIAN_POINT('Ctrl Pts',(-0.525262163586104,-0.705397811122471,
0.3661201878982));
#10029=CARTESIAN_POINT('Ctrl Pts',(-0.498886380082438,-0.739472435201248,
0.0605686695244023));
#10030=CARTESIAN_POINT('Ctrl Pts',(-0.493727440697609,-0.738921997925201,
0.000683776622396153));
#10031=CARTESIAN_POINT('Origin',(-5.57277255930238,0.,0.));
#10032=CARTESIAN_POINT('',(-1.37277255930238,-0.738120723810616,0.000490887946787387));
#10033=CARTESIAN_POINT('',(-1.29372744069761,-0.738351779650516,-0.000593827039684428));
#10034=CARTESIAN_POINT('',(-5.57277255930238,-0.739,-6.04325409642289E-14));
#10035=CARTESIAN_POINT('Ctrl Pts',(-1.37277255930238,-0.738120723810616,
0.000490887946787378));
#10036=CARTESIAN_POINT('Ctrl Pts',(-1.35933861299887,-0.737171704215717,
-0.155875611928105));
#10037=CARTESIAN_POINT('Ctrl Pts',(-1.32468782257652,-0.611933246648795,
-0.560587924185944));
#10038=CARTESIAN_POINT('Ctrl Pts',(-1.26882018803533,0.0542339661358782,
-0.872439386374161));
#10039=CARTESIAN_POINT('Ctrl Pts',(-1.20516965567882,0.763358611644189,
-0.42588194190445));
#10040=CARTESIAN_POINT('Ctrl Pts',(-1.1415191233223,0.770885820952385,0.412100544420447));
#10041=CARTESIAN_POINT('Ctrl Pts',(-1.07786859096579,0.0698973652520763,
0.871324379479602));
#10042=CARTESIAN_POINT('Ctrl Pts',(-1.02161973629248,-0.606347481192638,
0.569444027521707));
#10043=CARTESIAN_POINT('Ctrl Pts',(-0.986587725738014,-0.73713349877715,
0.160212366099622));
#10044=CARTESIAN_POINT('Ctrl Pts',(-0.972772559302383,-0.738215232575273,
-0.000539730860128814));
#10045=CARTESIAN_POINT('Ctrl Pts',(-1.29372744069761,-0.738351779650516,
-0.000593827039684532));
#10046=CARTESIAN_POINT('Ctrl Pts',(-1.28682184284182,-0.738953933815214,
-0.0809093790985889));
#10047=CARTESIAN_POINT('Ctrl Pts',(-1.25869940086719,-0.689800981336988,
-0.407270492702223));
#10048=CARTESIAN_POINT('Ctrl Pts',(-1.20936011477373,-0.212496869042399,
-0.847901434301904));
#10049=CARTESIAN_POINT('Ctrl Pts',(-1.14570958241722,0.59855736638473,-0.637040650488649));
#10050=CARTESIAN_POINT('Ctrl Pts',(-1.0820590500607,0.859481852719735,0.159319583000468));
#10051=CARTESIAN_POINT('Ctrl Pts',(-1.01840851770419,0.330462617873412,
0.809250439429974));
#10052=CARTESIAN_POINT('Ctrl Pts',(-0.955631314583161,-0.490856437121907,
0.716692412779907));
#10053=CARTESIAN_POINT('Ctrl Pts',(-0.914070955580967,-0.739369165809196,
0.234925255563142));
#10054=CARTESIAN_POINT('Ctrl Pts',(-0.89372744069761,-0.740166066981926,
-0.000187398345083168));
#10055=CARTESIAN_POINT('Origin',(-5.57277255930238,0.,0.));
#10056=CARTESIAN_POINT('',(-1.77277255930238,-0.74001018118917,0.000359371193499534));
#10057=CARTESIAN_POINT('',(-1.69372744069761,-0.738012890929405,0.000418943920021259));
#10058=CARTESIAN_POINT('',(-5.57277255930238,-0.739,-6.04325409642289E-14));
#10059=CARTESIAN_POINT('Ctrl Pts',(-1.77277255930238,-0.74001018118917,
0.000359371193499598));
#10060=CARTESIAN_POINT('Ctrl Pts',(-1.75330634437856,-0.738665492432069,
-0.224740083076168));
#10061=CARTESIAN_POINT('Ctrl Pts',(-1.7126232853359,-0.508643526817856,
-0.6975598184478));
#10062=CARTESIAN_POINT('Ctrl Pts',(-1.6507233821744,0.296733987625408,-0.822216969261532));
#10063=CARTESIAN_POINT('Ctrl Pts',(-1.58707284981789,0.852162790879889,
-0.194705884945239));
#10064=CARTESIAN_POINT('Ctrl Pts',(-1.52342231746138,0.624374863149558,
0.611757986611301));
#10065=CARTESIAN_POINT('Ctrl Pts',(-1.45977178510486,-0.177271539587102,
0.85595946486723));
#10066=CARTESIAN_POINT('Ctrl Pts',(-1.40955519905187,-0.681182597955438,
0.427954616763965));
#10067=CARTESIAN_POINT('Ctrl Pts',(-1.38055545711771,-0.738670534146682,
0.0910811331934603));
#10068=CARTESIAN_POINT('Ctrl Pts',(-1.37277255930238,-0.738120723810616,
0.000490887946787378));
#10069=CARTESIAN_POINT('Ctrl Pts',(-1.69372744069761,-0.738012890929405,
0.000418943920021233));
#10070=CARTESIAN_POINT('Ctrl Pts',(-1.68078957422151,-0.737239737698494,
-0.150228476501734));
#10071=CARTESIAN_POINT('Ctrl Pts',(-1.64663486362657,-0.619020886363836,
-0.549037359237818));
#10072=CARTESIAN_POINT('Ctrl Pts',(-1.5912633089128,0.0338258031167203,
-0.873468697178942));
#10073=CARTESIAN_POINT('Ctrl Pts',(-1.52761277655629,0.753194985694247,
-0.4436091323606));
#10074=CARTESIAN_POINT('Ctrl Pts',(-1.46396224419978,0.780308040630171,
0.393968414505714));
#10075=CARTESIAN_POINT('Ctrl Pts',(-1.40031171184326,0.0902455498640702,
0.869452409496697));
#10076=CARTESIAN_POINT('Ctrl Pts',(-1.34356677734254,-0.598895657855919,
0.580939588736018));
#10077=CARTESIAN_POINT('Ctrl Pts',(-1.30803868696066,-0.737103867924512,
0.165853114741589));
#10078=CARTESIAN_POINT('Ctrl Pts',(-1.29372744069761,-0.738351779650516,
-0.000593827039684532));
#10079=CARTESIAN_POINT('Origin',(-5.57277255930238,0.,0.));
#10080=CARTESIAN_POINT('',(-2.17277255930238,-0.739233177974631,-0.000663082281737704));
#10081=CARTESIAN_POINT('',(-2.09372744069761,-0.739887975806137,0.000444318217750006));
#10082=CARTESIAN_POINT('',(-5.57277255930238,-0.739,-6.04325409642289E-14));
#10083=CARTESIAN_POINT('Ctrl Pts',(-2.17277255930238,-0.739233177974631,
-0.000663082281737804));
#10084=CARTESIAN_POINT('Ctrl Pts',(-2.16849091987709,-0.739693649128342,
-0.0503097926539292));
#10085=CARTESIAN_POINT('Ctrl Pts',(-2.14299243633295,-0.712465622852962,
-0.345468936269266));
#10086=CARTESIAN_POINT('Ctrl Pts',(-2.09627710866998,-0.31545146146759,
-0.815219098988737));
#10087=CARTESIAN_POINT('Ctrl Pts',(-2.03262657631347,0.515417152562384,
-0.706000681829764));
#10088=CARTESIAN_POINT('Ctrl Pts',(-1.96897604395696,0.872569545068786,
0.0520979166081116));
#10089=CARTESIAN_POINT('Ctrl Pts',(-1.90532551160045,0.427749504473617,
0.762313692202795));
#10090=CARTESIAN_POINT('Ctrl Pts',(-1.84167497924393,-0.410212048803786,
0.771892401130592));
#10091=CARTESIAN_POINT('Ctrl Pts',(-1.79749066181125,-0.730181988681622,
0.286068839457169));
#10092=CARTESIAN_POINT('Ctrl Pts',(-1.7745231884974,-0.74013111129323,0.0206029407815301));
#10093=CARTESIAN_POINT('Ctrl Pts',(-1.77277255930238,-0.74001018118917,
0.000359371193499598));
#10094=CARTESIAN_POINT('Ctrl Pts',(-2.09372744069761,-0.739887975806136,
0.000444318217749989));
#10095=CARTESIAN_POINT('Ctrl Pts',(-2.0747573056012,-0.738332505019238,
-0.219014122774023));
#10096=CARTESIAN_POINT('Ctrl Pts',(-2.03457032638595,-0.518380685702002,
-0.686629244064919));
#10097=CARTESIAN_POINT('Ctrl Pts',(-1.97316650305187,0.277433510738858,
-0.828928462950496));
#10098=CARTESIAN_POINT('Ctrl Pts',(-1.90951597069536,0.847378654460013,
-0.214572052031487));
#10099=CARTESIAN_POINT('Ctrl Pts',(-1.84586543833885,0.638504132631428,
0.596995998455636));
#10100=CARTESIAN_POINT('Ctrl Pts',(-1.78221490598233,-0.157214974508773,
0.859869293211175));
#10101=CARTESIAN_POINT('Ctrl Pts',(-1.73150224010192,-0.676068489805857,
0.43964970956266));
#10102=CARTESIAN_POINT('Ctrl Pts',(-1.70200641834035,-0.738507633886055,
0.0968186577300095));
#10103=CARTESIAN_POINT('Ctrl Pts',(-1.69372744069761,-0.738012890929405,
0.000418943920021233));
#10104=CARTESIAN_POINT('Origin',(-5.57277255930238,0.,0.));
#10105=CARTESIAN_POINT('',(-2.57277255930238,-0.737778532894652,-5.68139967608906E-5));
#10106=CARTESIAN_POINT('',(-2.49372744069761,-0.739406836446418,-0.000631112843053269));
#10107=CARTESIAN_POINT('',(-5.57277255930238,-0.739,-6.04325409642289E-14));
#10108=CARTESIAN_POINT('Ctrl Pts',(-2.57277255930238,-0.737778532894651,
-5.68139967609561E-5));
#10109=CARTESIAN_POINT('Ctrl Pts',(-2.56245865125678,-0.737860611962286,
-0.12024640403614));
#10110=CARTESIAN_POINT('Ctrl Pts',(-2.53092789909234,-0.65320604174484,
-0.487570229219569));
#10111=CARTESIAN_POINT('Ctrl Pts',(-2.47818030280905,-0.0741628352493615,
-0.870971685972771));
#10112=CARTESIAN_POINT('Ctrl Pts',(-2.41452977045254,0.692731220865135,
-0.533118429185269));
#10113=CARTESIAN_POINT('Ctrl Pts',(-2.35087923809603,0.822940962445597,
0.294720165966547));
#10114=CARTESIAN_POINT('Ctrl Pts',(-2.28722870573952,0.196791546541912,
0.851683562778987));
#10115=CARTESIAN_POINT('Ctrl Pts',(-2.2278598128083,-0.555941069403201,
0.64106064804113));
#10116=CARTESIAN_POINT('Ctrl Pts',(-2.18970776399592,-0.737411872519181,
0.195704971867495));
#10117=CARTESIAN_POINT('Ctrl Pts',(-2.17277255930238,-0.739233177974631,
-0.000663082281737804));
#10118=CARTESIAN_POINT('Ctrl Pts',(-2.49372744069761,-0.739406836446418,
-0.000631112843053248));
#10119=CARTESIAN_POINT('Ctrl Pts',(-2.48994188109973,-0.739804758774596,
-0.044499082939427));
#10120=CARTESIAN_POINT('Ctrl Pts',(-2.46493947738301,-0.71624807112371,
-0.333806148989968));
#10121=CARTESIAN_POINT('Ctrl Pts',(-2.41872022954745,-0.334421070564838,
-0.807622620488002));
#10122=CARTESIAN_POINT('Ctrl Pts',(-2.35506969719094,0.49877348127123,-0.717855670690444));
#10123=CARTESIAN_POINT('Ctrl Pts',(-2.29141916483443,0.873548890926182,
0.0316872959253779));
#10124=CARTESIAN_POINT('Ctrl Pts',(-2.22776863247792,0.445451757697473,
0.752106695307021));
#10125=CARTESIAN_POINT('Ctrl Pts',(-2.16411810012141,-0.392056902636943,
0.781270205919639));
#10126=CARTESIAN_POINT('Ctrl Pts',(-2.11943770286131,-0.727014554612505,
0.29768960487206));
#10127=CARTESIAN_POINT('Ctrl Pts',(-2.09597414972004,-0.74007219643679,
0.0264356597089086));
#10128=CARTESIAN_POINT('Ctrl Pts',(-2.09372744069761,-0.739887975806136,
0.000444318217749989));
#10129=CARTESIAN_POINT('Origin',(-5.57277255930238,0.,0.));
#10130=CARTESIAN_POINT('',(-2.97277255930238,-0.739023959462765,0.000682056737534574));
#10131=CARTESIAN_POINT('',(-2.89372744069761,-0.737802707301305,-0.000151456297486224));
#10132=CARTESIAN_POINT('',(-5.57277255930238,-0.739,-6.04325409642289E-14));
#10133=CARTESIAN_POINT('Ctrl Pts',(-2.97277255930239,-0.739023959462765,
0.000682056737534627));
#10134=CARTESIAN_POINT('Ctrl Pts',(-2.95642638263647,-0.737265664930682,
-0.188993669098672));
#10135=CARTESIAN_POINT('Ctrl Pts',(-2.91886336185172,-0.566111381187521,
-0.62768042869388));
#10136=CARTESIAN_POINT('Ctrl Pts',(-2.86008349694812,0.173078347037689,
-0.856817185689954));
#10137=CARTESIAN_POINT('Ctrl Pts',(-2.79643296459162,0.814444375048807,
-0.317446316483022));
#10138=CARTESIAN_POINT('Ctrl Pts',(-2.7327824322351,0.707260398330102,0.513687193582241));
#10139=CARTESIAN_POINT('Ctrl Pts',(-2.66913189987859,-0.0499615560978463,
0.872694475066671));
#10140=CARTESIAN_POINT('Ctrl Pts',(-2.61579527556768,-0.646004991358073,
0.50141101156326));
#10141=CARTESIAN_POINT('Ctrl Pts',(-2.58367549537561,-0.737691766285582,
0.126996812143099));
#10142=CARTESIAN_POINT('Ctrl Pts',(-2.57277255930238,-0.737778532894651,
-5.68139967609561E-5));
#10143=CARTESIAN_POINT('Ctrl Pts',(-2.89372744069761,-0.737802707301305,
-0.000151456297486372));
#10144=CARTESIAN_POINT('Ctrl Pts',(-2.88390961247942,-0.738011369865057,
-0.114550791237915));
#10145=CARTESIAN_POINT('Ctrl Pts',(-2.85287494014239,-0.659064530805607,
-0.475900365227651));
#10146=CARTESIAN_POINT('Ctrl Pts',(-2.80062342368653,-0.0945016025569013,
-0.869000113162917));
#10147=CARTESIAN_POINT('Ctrl Pts',(-2.73697289133001,0.680080231616739,
-0.549165392323239));
#10148=CARTESIAN_POINT('Ctrl Pts',(-2.6733223589735,0.829605185064603,0.275403316020986));
#10149=CARTESIAN_POINT('Ctrl Pts',(-2.60967182661699,0.216645941644821,
0.846850804764733));
#10150=CARTESIAN_POINT('Ctrl Pts',(-2.54980685385836,-0.547133472195477,
0.652268195747027));
#10151=CARTESIAN_POINT('Ctrl Pts',(-2.51115872521857,-0.737574532096065,
0.20136678161214));
#10152=CARTESIAN_POINT('Ctrl Pts',(-2.49372744069761,-0.739406836446418,
-0.000631112843053248));
#10153=CARTESIAN_POINT('Origin',(-5.57277255930238,0.,0.));
#10154=CARTESIAN_POINT('',(-3.37277255930238,-0.740124450588434,-0.000246465757174322));
#10155=CARTESIAN_POINT('',(-3.29372744069761,-0.738849286492114,0.000682051891756977));
#10156=CARTESIAN_POINT('',(-5.57277255930238,-0.739,-6.04325409642289E-14));
#10157=CARTESIAN_POINT('Ctrl Pts',(-3.37277255930238,-0.740124450588434,
-0.000246465757174463));
#10158=CARTESIAN_POINT('Ctrl Pts',(-3.371610958135,-0.740182554157143,-0.0136732529463693));
#10159=CARTESIAN_POINT('Ctrl Pts',(-3.34923251284877,-0.733756016290406,
-0.272285851888853));
#10160=CARTESIAN_POINT('Ctrl Pts',(-3.30563722344371,-0.431476922874065,
-0.760210147363717));
#10161=CARTESIAN_POINT('Ctrl Pts',(-3.2419866910872,0.406427684917135,-0.773891685687522));
#10162=CARTESIAN_POINT('Ctrl Pts',(-3.17833615873069,0.870787512154351,
-0.0762949054116745));
#10163=CARTESIAN_POINT('Ctrl Pts',(-3.11468562637417,0.534812759927923,
0.691423976739877));
#10164=CARTESIAN_POINT('Ctrl Pts',(-3.05103509401767,-0.292704577900781,
0.82366002332857));
#10165=CARTESIAN_POINT('Ctrl Pts',(-3.00373073832707,-0.707771486157191,
0.359327625424719));
#10166=CARTESIAN_POINT('Ctrl Pts',(-2.97764322675531,-0.73954787818242,
0.0571997001792664));
#10167=CARTESIAN_POINT('Ctrl Pts',(-2.97277255930239,-0.739023959462765,
0.000682056737534627));
#10168=CARTESIAN_POINT('Ctrl Pts',(-3.29372744069761,-0.738849286492114,
0.000682051891756951));
#10169=CARTESIAN_POINT('Ctrl Pts',(-3.27787734385911,-0.737179572704079,
-0.183348274198659));
#10170=CARTESIAN_POINT('Ctrl Pts',(-3.24081040290178,-0.574437187223162,
-0.616355127026407));
#10171=CARTESIAN_POINT('Ctrl Pts',(-3.1825266178256,0.153002878688314,-0.860628763596925));
#10172=CARTESIAN_POINT('Ctrl Pts',(-3.11887608546909,0.806801478364629,
-0.336397271195981));
#10173=CARTESIAN_POINT('Ctrl Pts',(-3.05522555311257,0.719074605013923,
0.497014549054184));
#10174=CARTESIAN_POINT('Ctrl Pts',(-2.99157502075607,-0.0295485989689898,
0.873623849187583));
#10175=CARTESIAN_POINT('Ctrl Pts',(-2.93774231661774,-0.639730894183085,
0.513051660515881));
#10176=CARTESIAN_POINT('Ctrl Pts',(-2.90512645659826,-0.737560439069551,
0.132672199711606));
#10177=CARTESIAN_POINT('Ctrl Pts',(-2.89372744069761,-0.737802707301305,
-0.000151456297486372));
#10178=CARTESIAN_POINT('Origin',(-5.57277255930238,0.,0.));
#10179=CARTESIAN_POINT('',(-3.77277255930239,-0.738270663189668,-0.000563756901791942));
#10180=CARTESIAN_POINT('',(-3.69372744069761,-0.740189453003445,-0.000143777948279911));
#10181=CARTESIAN_POINT('',(-5.57277255930238,-0.739,-6.04325409642289E-14));
#10182=CARTESIAN_POINT('Ctrl Pts',(-3.77277255930239,-0.738270663189668,
-0.000563756901791916));
#10183=CARTESIAN_POINT('Ctrl Pts',(-3.76557868951469,-0.738861876141626,
-0.0842552170796602));
#10184=CARTESIAN_POINT('Ctrl Pts',(-3.73716797560816,-0.687028401393337,
-0.414066937544982));
#10185=CARTESIAN_POINT('Ctrl Pts',(-3.68754041758278,-0.200959315114973,
-0.850709773850142));
#10186=CARTESIAN_POINT('Ctrl Pts',(-3.62388988522628,0.607155781861951,
-0.628851073384074));
#10187=CARTESIAN_POINT('Ctrl Pts',(-3.56023935286976,0.857238345345858,
0.170980194542391));
#10188=CARTESIAN_POINT('Ctrl Pts',(-3.49658882051325,0.319439268341143,
0.813664766506036));
#10189=CARTESIAN_POINT('Ctrl Pts',(-3.43409988932412,-0.496781500447376,
0.71043480993338));
#10190=CARTESIAN_POINT('Ctrl Pts',(-3.39282780225383,-0.739121282530827,
0.231569312925605));
#10191=CARTESIAN_POINT('Ctrl Pts',(-3.37277255930238,-0.740124450588434,
-0.000246465757174463));
#10192=CARTESIAN_POINT('Ctrl Pts',(-3.69372744069761,-0.740189453003445,
-0.000143777948279917));
#10193=CARTESIAN_POINT('Ctrl Pts',(-3.69306191935764,-0.740209898516256,
-0.00783464190255628));
#10194=CARTESIAN_POINT('Ctrl Pts',(-3.67117955389883,-0.736611233978934,
-0.260690917954438));
#10195=CARTESIAN_POINT('Ctrl Pts',(-3.62808034432118,-0.449128986023828,
-0.749916594011252));
#10196=CARTESIAN_POINT('Ctrl Pts',(-3.56442981196467,0.388226838966437,
-0.78318048568386));
#10197=CARTESIAN_POINT('Ctrl Pts',(-3.50077927960816,0.868766152624766,
-0.0966287842922777));
#10198=CARTESIAN_POINT('Ctrl Pts',(-3.43712874725165,0.550828702979369,
0.678733739225294));
#10199=CARTESIAN_POINT('Ctrl Pts',(-3.37347821489513,-0.273371470575397,
0.830276935114671));
#10200=CARTESIAN_POINT('Ctrl Pts',(-3.32567777937712,-0.703644193492458,
0.37100728094817));
#10201=CARTESIAN_POINT('Ctrl Pts',(-3.29909418797795,-0.739414641519417,
0.0629936113799137));
#10202=CARTESIAN_POINT('Ctrl Pts',(-3.29372744069761,-0.738849286492114,
0.000682051891756951));
#10203=CARTESIAN_POINT('Origin',(-5.57277255930238,0.,0.));
#10204=CARTESIAN_POINT('',(-4.17277255930238,-0.738073231265952,0.00046280520781095));
#10205=CARTESIAN_POINT('',(-4.09372744069761,-0.73841309200618,-0.000613006299877497));
#10206=CARTESIAN_POINT('',(-5.57277255930238,-0.739,-6.04325409642289E-14));
#10207=CARTESIAN_POINT('Ctrl Pts',(-4.17277255930238,-0.738073231265952,
0.000462805207810824));
#10208=CARTESIAN_POINT('Ctrl Pts',(-4.15954642089438,-0.737197697708417,
-0.153510013395393));
#10209=CARTESIAN_POINT('Ctrl Pts',(-4.12510343836753,-0.614927323108488,
-0.555754388202545));
#10210=CARTESIAN_POINT('Ctrl Pts',(-4.06944361172186,0.045688116659549,
-0.872927632797439));
#10211=CARTESIAN_POINT('Ctrl Pts',(-4.00579307936534,0.759151449841031,
-0.433337290821689));
#10212=CARTESIAN_POINT('Ctrl Pts',(-3.94214254700883,0.774884419432483,
0.404532123885857));
#10213=CARTESIAN_POINT('Ctrl Pts',(-3.87849201465232,0.0784264940929817,
0.870597971361873));
#10214=CARTESIAN_POINT('Ctrl Pts',(-3.8220353520835,-0.60325124419292,0.574263722611057));
#10215=CARTESIAN_POINT('Ctrl Pts',(-3.78679553363353,-0.737118214744782,
0.162575587073693));
#10216=CARTESIAN_POINT('Ctrl Pts',(-3.77277255930239,-0.738270663189668,
-0.000563756901791916));
#10217=CARTESIAN_POINT('Ctrl Pts',(-4.09372744069761,-0.73841309200618,
-0.000613006299877436));
#10218=CARTESIAN_POINT('Ctrl Pts',(-4.08702965073733,-0.739019449463923,
-0.078495381476594));
#10219=CARTESIAN_POINT('Ctrl Pts',(-4.05911501665821,-0.691764139783589,
-0.402371677365512));
#10220=CARTESIAN_POINT('Ctrl Pts',(-4.00998353846026,-0.220789764456959,
-0.845779739504579));
#10221=CARTESIAN_POINT('Ctrl Pts',(-3.94633300610374,0.592290396078366,
-0.642871606343513));
#10222=CARTESIAN_POINT('Ctrl Pts',(-3.88268247374723,0.861000775993609,
0.150895488403042));
#10223=CARTESIAN_POINT('Ctrl Pts',(-3.81903194139071,0.33837144853579,0.805975479803333));
#10224=CARTESIAN_POINT('Ctrl Pts',(-3.75604693037418,-0.486536373785569,
0.721185164181757));
#10225=CARTESIAN_POINT('Ctrl Pts',(-3.71427876347648,-0.739558094836668,
0.237350376002131));
#10226=CARTESIAN_POINT('Ctrl Pts',(-3.69372744069761,-0.740189453003445,
-0.000143777948279917));
#10227=CARTESIAN_POINT('Origin',(-5.57277255930238,0.,0.));
#10228=CARTESIAN_POINT('',(-4.57277255930238,-0.73995294767526,0.000448391410152922));
#10229=CARTESIAN_POINT('',(-4.49372744069761,-0.73797111367679,0.000392387352095118));
#10230=CARTESIAN_POINT('',(-5.57277255930238,-0.739,-6.04325409642289E-14));
#10231=CARTESIAN_POINT('Ctrl Pts',(-4.57277255930238,-0.73995294767526,
0.000448391410152972));
#10232=CARTESIAN_POINT('Ctrl Pts',(-4.55351415227407,-0.73850922179247,
-0.22227076833447));
#10233=CARTESIAN_POINT('Ctrl Pts',(-4.51303890112692,-0.512764590101588,
-0.693075680093264));
#10234=CARTESIAN_POINT('Ctrl Pts',(-4.45134680586093,0.28867595279949,-0.825036182879565));
#10235=CARTESIAN_POINT('Ctrl Pts',(-4.38769627350442,0.850211150606986,
-0.203066249722066));
#10236=CARTESIAN_POINT('Ctrl Pts',(-4.3240457411479,0.63033776882184,0.605627518939458));
#10237=CARTESIAN_POINT('Ctrl Pts',(-4.2603952087914,-0.168882147113114,
0.85764746510496));
#10238=CARTESIAN_POINT('Ctrl Pts',(-4.20997081484289,-0.679061471453575,
0.432855387436826));
#10239=CARTESIAN_POINT('Ctrl Pts',(-4.18076326501322,-0.73860219374785,
0.0934870457662381));
#10240=CARTESIAN_POINT('Ctrl Pts',(-4.17277255930238,-0.738073231265952,
0.000462805207810824));
#10241=CARTESIAN_POINT('Ctrl Pts',(-4.49372744069761,-0.73797111367679,
0.000392387352095092));
#10242=CARTESIAN_POINT('Ctrl Pts',(-4.48099738211702,-0.73727274911154,
-0.147857884919729));
#10243=CARTESIAN_POINT('Ctrl Pts',(-4.44705047941759,-0.621933032261733,
-0.544200764147008));
#10244=CARTESIAN_POINT('Ctrl Pts',(-4.39188673259933,0.0252729501941139,
-0.87375143017453));
#10245=CARTESIAN_POINT('Ctrl Pts',(-4.32823620024282,0.748813609559634,
-0.450967062073938));
#10246=CARTESIAN_POINT('Ctrl Pts',(-4.2645856678863,0.784129213744664,0.386310152740616));
#10247=CARTESIAN_POINT('Ctrl Pts',(-4.20093513552979,0.0987550571481419,
0.86852601426748));
#10248=CARTESIAN_POINT('Ctrl Pts',(-4.14398239313356,-0.595711893577857,
0.585745002940476));
#10249=CARTESIAN_POINT('Ctrl Pts',(-4.10824649485617,-0.737098667872156,
0.168215581920015));
#10250=CARTESIAN_POINT('Ctrl Pts',(-4.09372744069761,-0.73841309200618,
-0.000613006299877436));
#10251=CARTESIAN_POINT('Ctrl Pts',(-4.96474152380793,-0.324968229607127,
0.663714283216814));
#10252=CARTESIAN_POINT('Ctrl Pts',(-4.9435246796891,-0.546166550766499,
0.555411013817762));
#10253=CARTESIAN_POINT('Ctrl Pts',(-4.90109099145142,-0.8678824284367,0.102108364545744));
#10254=CARTESIAN_POINT('Ctrl Pts',(-4.83744045909491,-0.554348105578856,
-0.676628674894764));
#10255=CARTESIAN_POINT('Ctrl Pts',(-4.7737899267384,0.269408751288173,-0.831294757094915));
#10256=CARTESIAN_POINT('Ctrl Pts',(-4.71013939438189,0.845181125686649,
-0.223022892376799));
#10257=CARTESIAN_POINT('Ctrl Pts',(-4.64648886202537,0.644348974298595,
0.590800680695443));
#10258=CARTESIAN_POINT('Ctrl Pts',(-4.58283832966888,-0.148802575908472,
0.861322337488271));
#10259=CARTESIAN_POINT('Ctrl Pts',(-4.51918779731234,-0.805136543447083,
0.340367467401713));
#10260=CARTESIAN_POINT('Ctrl Pts',(-4.45553726495584,-0.721503831726609,
-0.493500331564431));
#10261=CARTESIAN_POINT('Ctrl Pts',(-4.39188673259933,0.0252729501941139,
-0.87375143017453));
#10262=CARTESIAN_POINT('Ctrl Pts',(-4.32823620024282,0.748813609559634,
-0.450967062073938));
#10263=CARTESIAN_POINT('Ctrl Pts',(-4.2645856678863,0.784129213744664,0.386310152740616));
#10264=CARTESIAN_POINT('Ctrl Pts',(-4.20093513552979,0.0987550571481419,
0.86852601426748));
#10265=CARTESIAN_POINT('Ctrl Pts',(-4.13728460317328,-0.677383005004931,
0.552489223869342));
#10266=CARTESIAN_POINT('Ctrl Pts',(-4.07363407081676,-0.830943800430228,
-0.271338256335547));
#10267=CARTESIAN_POINT('Ctrl Pts',(-4.00998353846026,-0.220789764456959,
-0.845779739504579));
#10268=CARTESIAN_POINT('Ctrl Pts',(-3.94633300610374,0.592290396078366,
-0.642871606343513));
#10269=CARTESIAN_POINT('Ctrl Pts',(-3.88268247374723,0.861000775993609,
0.150895488403042));
#10270=CARTESIAN_POINT('Ctrl Pts',(-3.81903194139071,0.33837144853579,0.805975479803333));
#10271=CARTESIAN_POINT('Ctrl Pts',(-3.75538140903421,-0.495252634216496,
0.720289240476126));
#10272=CARTESIAN_POINT('Ctrl Pts',(-3.69173087667769,-0.87369357327973,
-0.0274097306918623));
#10273=CARTESIAN_POINT('Ctrl Pts',(-3.62808034432118,-0.449128986023828,
-0.749916594011252));
#10274=CARTESIAN_POINT('Ctrl Pts',(-3.56442981196467,0.388226838966437,
-0.78318048568386));
#10275=CARTESIAN_POINT('Ctrl Pts',(-3.50077927960816,0.868766152624766,
-0.0966287842922777));
#10276=CARTESIAN_POINT('Ctrl Pts',(-3.43712874725165,0.550828702979369,
0.678733739225294));
#10277=CARTESIAN_POINT('Ctrl Pts',(-3.37347821489513,-0.273371470575397,
0.830276935114671));
#10278=CARTESIAN_POINT('Ctrl Pts',(-3.30982768253862,-0.846317879438916,
0.218718532642087));
#10279=CARTESIAN_POINT('Ctrl Pts',(-3.24617715018211,-0.641419573323106,
-0.593862509688507));
#10280=CARTESIAN_POINT('Ctrl Pts',(-3.1825266178256,0.153002878688314,-0.860628763596925));
#10281=CARTESIAN_POINT('Ctrl Pts',(-3.11887608546909,0.806801478364629,
-0.336397271195981));
#10282=CARTESIAN_POINT('Ctrl Pts',(-3.05522555311257,0.719074605013923,
0.497014549054184));
#10283=CARTESIAN_POINT('Ctrl Pts',(-2.99157502075607,-0.0295485989689898,
0.873623849187583));
#10284=CARTESIAN_POINT('Ctrl Pts',(-2.92792448839955,-0.751013896812873,
0.447291712816805));
#10285=CARTESIAN_POINT('Ctrl Pts',(-2.86427395604304,-0.782227689169792,
-0.390143040250507));
#10286=CARTESIAN_POINT('Ctrl Pts',(-2.80062342368653,-0.0945016025569013,
-0.869000113162917));
#10287=CARTESIAN_POINT('Ctrl Pts',(-2.73697289133001,0.680080231616739,
-0.549165392323239));
#10288=CARTESIAN_POINT('Ctrl Pts',(-2.6733223589735,0.829605185064603,0.275403316020986));
#10289=CARTESIAN_POINT('Ctrl Pts',(-2.60967182661699,0.216645941644821,
0.846850804764733));
#10290=CARTESIAN_POINT('Ctrl Pts',(-2.54602129426048,-0.5954310384933,0.639963770818652));
#10291=CARTESIAN_POINT('Ctrl Pts',(-2.48237076190397,-0.860251606365249,
-0.155109391423006));
#10292=CARTESIAN_POINT('Ctrl Pts',(-2.41872022954745,-0.334421070564838,
-0.807622620488002));
#10293=CARTESIAN_POINT('Ctrl Pts',(-2.35506969719094,0.49877348127123,-0.717855670690444));
#10294=CARTESIAN_POINT('Ctrl Pts',(-2.29141916483443,0.873548890926182,
0.0316872959253779));
#10295=CARTESIAN_POINT('Ctrl Pts',(-2.22776863247792,0.445451757697473,
0.752106695307021));
#10296=CARTESIAN_POINT('Ctrl Pts',(-2.16411810012141,-0.392056902636943,
0.781270205919639));
#10297=CARTESIAN_POINT('Ctrl Pts',(-2.1004675677649,-0.869228865567758,
0.0923738535712786));
#10298=CARTESIAN_POINT('Ctrl Pts',(-2.03681703540838,-0.547498790051825,
-0.681422647446086));
#10299=CARTESIAN_POINT('Ctrl Pts',(-1.97316650305187,0.277433510738858,
-0.828928462950496));
#10300=CARTESIAN_POINT('Ctrl Pts',(-1.90951597069536,0.847378654460013,
-0.214572052031487));
#10301=CARTESIAN_POINT('Ctrl Pts',(-1.84586543833885,0.638504132631428,
0.596995998455636));
#10302=CARTESIAN_POINT('Ctrl Pts',(-1.78221490598233,-0.157214974508773,
0.859869293211175));
#10303=CARTESIAN_POINT('Ctrl Pts',(-1.71856437362582,-0.808438922024868,
0.332442865483368));
#10304=CARTESIAN_POINT('Ctrl Pts',(-1.65491384126931,-0.716632433922576,
-0.500529423939589));
#10305=CARTESIAN_POINT('Ctrl Pts',(-1.5912633089128,0.0338258031167203,
-0.873468697178942));
#10306=CARTESIAN_POINT('Ctrl Pts',(-1.52761277655629,0.753194985694247,
-0.4436091323606));
#10307=CARTESIAN_POINT('Ctrl Pts',(-1.46396224419978,0.780308040630171,
0.393968414505714));
#10308=CARTESIAN_POINT('Ctrl Pts',(-1.40031171184326,0.0902455498640702,
0.869452409496697));
#10309=CARTESIAN_POINT('Ctrl Pts',(-1.33666117948675,-0.682760977082029,
0.545828903809815));
#10310=CARTESIAN_POINT('Ctrl Pts',(-1.27301064713024,-0.828246776447871,
-0.279462037906061));
#10311=CARTESIAN_POINT('Ctrl Pts',(-1.20936011477373,-0.212496869042399,
-0.847901434301904));
#10312=CARTESIAN_POINT('Ctrl Pts',(-1.14570958241722,0.59855736638473,-0.637040650488649));
#10313=CARTESIAN_POINT('Ctrl Pts',(-1.0820590500607,0.859481852719735,0.159319583000468));
#10314=CARTESIAN_POINT('Ctrl Pts',(-1.01840851770419,0.330462617873412,
0.809250439429974));
#10315=CARTESIAN_POINT('Ctrl Pts',(-0.954757985347679,-0.502282271767681,
0.715404785637677));
#10316=CARTESIAN_POINT('Ctrl Pts',(-0.891107452991167,-0.873383448243801,
-0.0359638868646765));
#10317=CARTESIAN_POINT('Ctrl Pts',(-0.827456920634656,-0.441763506671353,
-0.754279180499295));
#10318=CARTESIAN_POINT('Ctrl Pts',(-0.763806388278142,0.395876917069436,
-0.779340403997693));
#10319=CARTESIAN_POINT('Ctrl Pts',(-0.700155855921632,0.869671971808336,
-0.0881182126992239));
#10320=CARTESIAN_POINT('Ctrl Pts',(-0.636505323565118,0.544153413313058,
0.68409807463336));
#10321=CARTESIAN_POINT('Ctrl Pts',(-0.572854791208608,-0.281484464039597,
0.827554699248267));
#10322=CARTESIAN_POINT('Ctrl Pts',(-0.509204258852095,-0.848427529862204,
0.210430708363356));
#10323=CARTESIAN_POINT('Ctrl Pts',(-0.445553726495583,-0.635557416936722,
-0.600134681747435));
#10324=CARTESIAN_POINT('Ctrl Pts',(-0.381903194139071,0.161393004974118,
-0.859052194921053));
#10325=CARTESIAN_POINT('Ctrl Pts',(-0.318252661782561,0.810114474683083,
-0.328550731088526));
#10326=CARTESIAN_POINT('Ctrl Pts',(-0.254602129426047,0.714063928013904,
0.504165699398937));
#10327=CARTESIAN_POINT('Ctrl Pts',(-0.190951597069536,-0.0378944583360208,
0.873038406069037));
#10328=CARTESIAN_POINT('Ctrl Pts',(-0.127301064713024,-0.755757544293365,
0.440407447816644));
#10329=CARTESIAN_POINT('Ctrl Pts',(-0.0636505323565111,-0.777566173241284,
-0.398794275197495));
#10330=CARTESIAN_POINT('Ctrl Pts',(-0.0212168441188374,-0.31778980334938,
-0.71118839721512));
#10331=CARTESIAN_POINT('Ctrl Pts',(0.,-0.0726952737146206,-0.735415798837336));
#10332=CARTESIAN_POINT('Ctrl Pts',(-4.92091101587196,-0.35835186257646,
0.73189693003803));
#10333=CARTESIAN_POINT('Ctrl Pts',(-4.89969417175312,-0.602273646813887,
0.61246778350518));
#10334=CARTESIAN_POINT('Ctrl Pts',(-4.85726048351545,-0.957039046874433,
0.112597845838169));
#10335=CARTESIAN_POINT('Ctrl Pts',(-4.79360995115893,-0.611295683858332,
-0.746138003134398));
#10336=CARTESIAN_POINT('Ctrl Pts',(-4.72995941880242,0.297084819445984,
-0.916692763828507));
#10337=CARTESIAN_POINT('Ctrl Pts',(-4.66630888644591,0.932005663970424,
-0.245933791672618));
#10338=CARTESIAN_POINT('Ctrl Pts',(-4.60265835408939,0.710542243985793,
0.651492992390695));
#10339=CARTESIAN_POINT('Ctrl Pts',(-4.53900782173289,-0.164088902775022,
0.949805044914052));
#10340=CARTESIAN_POINT('Ctrl Pts',(-4.47535728937636,-0.887847345328032,
0.375333047329884));
#10341=CARTESIAN_POINT('Ctrl Pts',(-4.41170675701986,-0.795623136045845,
-0.544197084164244));
#10342=CARTESIAN_POINT('Ctrl Pts',(-4.34805622466334,0.0278692128944719,
-0.963510964780867));
#10343=CARTESIAN_POINT('Ctrl Pts',(-4.28440569230684,0.825738417668429,
-0.49729441813499));
#10344=CARTESIAN_POINT('Ctrl Pts',(-4.22075515995032,0.864681955481405,
0.425995374791432));
#10345=CARTESIAN_POINT('Ctrl Pts',(-4.15710462759381,0.108900056816841,
0.957748747577997));
#10346=CARTESIAN_POINT('Ctrl Pts',(-4.0934540952373,-0.746969824756786,
0.609245841251504));
#10347=CARTESIAN_POINT('Ctrl Pts',(-4.02980356288079,-0.916305753767165,
-0.299212540449396));
#10348=CARTESIAN_POINT('Ctrl Pts',(-3.96615303052428,-0.243471256949106,
-0.932665772735145));
#10349=CARTESIAN_POINT('Ctrl Pts',(-3.90250249816777,0.653135744615505,
-0.708913107626664));
#10350=CARTESIAN_POINT('Ctrl Pts',(-3.83885196581125,0.949450449756597,
0.166396817895047));
#10351=CARTESIAN_POINT('Ctrl Pts',(-3.77520143345474,0.373131979615646,
0.888772464704192));
#10352=CARTESIAN_POINT('Ctrl Pts',(-3.71155090109823,-0.546129398962908,
0.794283771156525));
#10353=CARTESIAN_POINT('Ctrl Pts',(-3.64790036874171,-0.963447164310157,
-0.0302255025299563));
#10354=CARTESIAN_POINT('Ctrl Pts',(-3.58424983638521,-0.495267518530342,
-0.826954710513758));
#10355=CARTESIAN_POINT('Ctrl Pts',(-3.52059930402869,0.42810896010969,-0.863635765618234));
#10356=CARTESIAN_POINT('Ctrl Pts',(-3.45694877167218,0.958013555087683,
-0.106555354261868));
#10357=CARTESIAN_POINT('Ctrl Pts',(-3.39329823931567,0.607414736855583,
0.748459318435285));
#10358=CARTESIAN_POINT('Ctrl Pts',(-3.32964770695916,-0.301454624577893,
0.91557038210266));
#10359=CARTESIAN_POINT('Ctrl Pts',(-3.26599717460264,-0.933259195199948,
0.241187249741433));
#10360=CARTESIAN_POINT('Ctrl Pts',(-3.20234664224614,-0.707311908832511,
-0.654869359747841));
#10361=CARTESIAN_POINT('Ctrl Pts',(-3.13869610988962,0.168720698093478,
-0.9490402209308));
#10362=CARTESIAN_POINT('Ctrl Pts',(-3.07504557753311,0.889683317199782,
-0.370954997183757));
#10363=CARTESIAN_POINT('Ctrl Pts',(-3.01139504517659,0.792944357513666,
0.548072313396573));
#10364=CARTESIAN_POINT('Ctrl Pts',(-2.94774451282008,-0.0325840944201276,
0.963370277537819));
#10365=CARTESIAN_POINT('Ctrl Pts',(-2.88409398046357,-0.82816473803936,
0.493241504243977));
#10366=CARTESIAN_POINT('Ctrl Pts',(-2.82044344810706,-0.862585089354017,
-0.430222010668657));
#10367=CARTESIAN_POINT('Ctrl Pts',(-2.75679291575055,-0.104209649459179,
-0.958271550137592));
#10368=CARTESIAN_POINT('Ctrl Pts',(-2.69314238339404,0.749944134526393,
-0.605580556103857));
#10369=CARTESIAN_POINT('Ctrl Pts',(-2.62949185103753,0.914829623900177,
0.303695199297379));
#10370=CARTESIAN_POINT('Ctrl Pts',(-2.56584131868101,0.238901743724037,
0.933846867365168));
#10371=CARTESIAN_POINT('Ctrl Pts',(-2.50219078632451,-0.656599021811674,
0.70570655331931));
#10372=CARTESIAN_POINT('Ctrl Pts',(-2.43854025396799,-0.948624318746706,
-0.171043610591511));
#10373=CARTESIAN_POINT('Ctrl Pts',(-2.37488972161148,-0.368775783610015,
-0.890588814360863));
#10374=CARTESIAN_POINT('Ctrl Pts',(-2.31123918925496,0.550011938808221,
-0.791600203392185));
#10375=CARTESIAN_POINT('Ctrl Pts',(-2.24758865689845,0.963287618895708,
0.0349424973899653));
#10376=CARTESIAN_POINT('Ctrl Pts',(-2.18393812454194,0.491212532535367,
0.82936979853488));
#10377=CARTESIAN_POINT('Ctrl Pts',(-2.12028759218543,-0.432332482057578,
0.861529244890413));
#10378=CARTESIAN_POINT('Ctrl Pts',(-2.05663705982892,-0.958523802028315,
0.101863319133242));
#10379=CARTESIAN_POINT('Ctrl Pts',(-1.9929865274724,-0.603742745592788,
-0.751424455274608));
#10380=CARTESIAN_POINT('Ctrl Pts',(-1.9293359951159,0.305933953711686,-0.914083382858923));
#10381=CARTESIAN_POINT('Ctrl Pts',(-1.86568546275938,0.934428942485842,
-0.236614805685157));
#10382=CARTESIAN_POINT('Ctrl Pts',(-1.80203493040287,0.704096968087819,
0.658324748409746));
#10383=CARTESIAN_POINT('Ctrl Pts',(-1.73838439804635,-0.173365497938794,
0.948202730977908));
#10384=CARTESIAN_POINT('Ctrl Pts',(-1.67473386568985,-0.891488973667248,
0.366594359670943));
#10385=CARTESIAN_POINT('Ctrl Pts',(-1.61108333333333,-0.790251304840878,
-0.551948267558096));
#10386=CARTESIAN_POINT('Ctrl Pts',(-1.54743280097682,0.0373006911003992,
-0.963199186931988));
#10387=CARTESIAN_POINT('Ctrl Pts',(-1.48378226862031,0.830569887810556,
-0.489180616300672));
#10388=CARTESIAN_POINT('Ctrl Pts',(-1.4201317362638,0.860468237406682,0.43444036146271));
#10389=CARTESIAN_POINT('Ctrl Pts',(-1.35648120390728,0.0995163770997762,
0.95877031038207));
#10390=CARTESIAN_POINT('Ctrl Pts',(-1.29283067155078,-0.752900270059216,
0.601901313752394));
#10391=CARTESIAN_POINT('Ctrl Pts',(-1.22918013919426,-0.913331667442913,
-0.308170869269657));
#10392=CARTESIAN_POINT('Ctrl Pts',(-1.16552960683775,-0.234326441403438,
-0.9350054269326));
#10393=CARTESIAN_POINT('Ctrl Pts',(-1.10187907448124,0.660046513968904,
-0.702483144015398));
#10394=CARTESIAN_POINT('Ctrl Pts',(-1.03822854212473,0.947775489145951,
0.175686310573016));
#10395=CARTESIAN_POINT('Ctrl Pts',(-0.974578009768212,0.364410683376652,
0.892383857373218));
#10396=CARTESIAN_POINT('Ctrl Pts',(-0.910927477411701,-0.553881183538126,
0.788897541582193));
#10397=CARTESIAN_POINT('Ctrl Pts',(-0.847276945055188,-0.963105180466411,
-0.03965841786757));
#10398=CARTESIAN_POINT('Ctrl Pts',(-0.783626412698676,-0.487145391490666,
-0.831765460769347));
#10399=CARTESIAN_POINT('Ctrl Pts',(-0.719975880342164,0.436544922420158,
-0.859401196514826));
#10400=CARTESIAN_POINT('Ctrl Pts',(-0.656325347985653,0.959012428091307,
-0.0971705009005156));
#10401=CARTESIAN_POINT('Ctrl Pts',(-0.59267481562914,0.600053701938256,
0.754374726188497));
#10402=CARTESIAN_POINT('Ctrl Pts',(-0.529024283272629,-0.310401057041403,
0.912568493904919));
#10403=CARTESIAN_POINT('Ctrl Pts',(-0.465373750916116,-0.935585567717916,
0.232048026283865));
#10404=CARTESIAN_POINT('Ctrl Pts',(-0.401723218559605,-0.700847539493036,
-0.66178586522419));
#10405=CARTESIAN_POINT('Ctrl Pts',(-0.338072686203092,0.177972732932097,
-0.947301693068673));
#10406=CARTESIAN_POINT('Ctrl Pts',(-0.274422153846582,0.893336654028625,
-0.36230239054068));
#10407=CARTESIAN_POINT('Ctrl Pts',(-0.210771621490068,0.787418939112313,
0.555958093642551));
#10408=CARTESIAN_POINT('Ctrl Pts',(-0.147121089133556,-0.0417873148475276,
0.962724692484114));
#10409=CARTESIAN_POINT('Ctrl Pts',(-0.0834705567770454,-0.833395695268921,
0.485650026183921));
#10410=CARTESIAN_POINT('Ctrl Pts',(-0.019820024420532,-0.857444700961496,
-0.439761977577384));
#10411=CARTESIAN_POINT('Ctrl Pts',(0.0226136638171417,-0.350436004392607,
-0.784248008160423));
#10412=CARTESIAN_POINT('Ctrl Pts',(0.0438305079359791,-0.0801631801595997,
-0.810964264414784));
#10413=CARTESIAN_POINT('Ctrl Pts',(-4.87708050793598,-0.391735495545793,
0.800079576859246));
#10414=CARTESIAN_POINT('Ctrl Pts',(-4.85586366381714,-0.658380742861275,
0.669524553192597));
#10415=CARTESIAN_POINT('Ctrl Pts',(-4.81342997557946,-1.04619566531217,
0.123087327130596));
#10416=CARTESIAN_POINT('Ctrl Pts',(-4.74977944322295,-0.668243262137807,
-0.815647331374034));
#10417=CARTESIAN_POINT('Ctrl Pts',(-4.68612891086644,0.324760887603795,
-1.0020907705621));
#10418=CARTESIAN_POINT('Ctrl Pts',(-4.62247837850992,1.0188302022542,-0.268844690968438));
#10419=CARTESIAN_POINT('Ctrl Pts',(-4.55882784615342,0.77673551367299,0.712185304085948));
#10420=CARTESIAN_POINT('Ctrl Pts',(-4.4951773137969,-0.17937522964157,1.03828775233983));
#10421=CARTESIAN_POINT('Ctrl Pts',(-4.43152678144039,-0.970558147208983,
0.410298627258055));
#10422=CARTESIAN_POINT('Ctrl Pts',(-4.36787624908388,-0.869742440365079,
-0.594893836764057));
#10423=CARTESIAN_POINT('Ctrl Pts',(-4.30422571672737,0.0304654755948294,
-1.0532704993872));
#10424=CARTESIAN_POINT('Ctrl Pts',(-4.24057518437085,0.902663225777224,
-0.543621774196043));
#10425=CARTESIAN_POINT('Ctrl Pts',(-4.17692465201435,0.945234697218146,
0.46568059684225));
#10426=CARTESIAN_POINT('Ctrl Pts',(-4.11327411965783,0.11904505648554,1.04697148088851));
#10427=CARTESIAN_POINT('Ctrl Pts',(-4.04962358730132,-0.816556644508641,
0.666002458633668));
#10428=CARTESIAN_POINT('Ctrl Pts',(-3.98597305494481,-1.0016677071041,-0.327086824563246));
#10429=CARTESIAN_POINT('Ctrl Pts',(-3.9223225225883,-0.266152749441253,
-1.01955180596571));
#10430=CARTESIAN_POINT('Ctrl Pts',(-3.85867199023178,0.713981093152643,
-0.774954608909815));
#10431=CARTESIAN_POINT('Ctrl Pts',(-3.79502145787528,1.03790012351959,0.181898147387054));
#10432=CARTESIAN_POINT('Ctrl Pts',(-3.73137092551876,0.407892510695502,
0.971569449605049));
#10433=CARTESIAN_POINT('Ctrl Pts',(-3.66772039316225,-0.597006163709318,
0.868278301836927));
#10434=CARTESIAN_POINT('Ctrl Pts',(-3.60406986080573,-1.05320075534059,
-0.0330412743680517));
#10435=CARTESIAN_POINT('Ctrl Pts',(-3.54041932844923,-0.541406051036855,
-0.903992827016263));
#10436=CARTESIAN_POINT('Ctrl Pts',(-3.47676879609271,0.467991081252941,
-0.944091045552607));
#10437=CARTESIAN_POINT('Ctrl Pts',(-3.4131182637362,1.0472609575506,-0.116481924231459));
#10438=CARTESIAN_POINT('Ctrl Pts',(-3.34946773137969,0.664000770731795,
0.818184897645276));
#10439=CARTESIAN_POINT('Ctrl Pts',(-3.28581719902317,-0.329537778580387,
1.00086382909065));
#10440=CARTESIAN_POINT('Ctrl Pts',(-3.22216666666667,-1.02020051096098,
0.263655966840779));
#10441=CARTESIAN_POINT('Ctrl Pts',(-3.15851613431015,-0.773204244341915,
-0.715876209807176));
#10442=CARTESIAN_POINT('Ctrl Pts',(-3.09486560195364,0.184438517498642,
-1.03745167826468));
#10443=CARTESIAN_POINT('Ctrl Pts',(-3.03121506959713,0.972565156034937,
-0.405512723171533));
#10444=CARTESIAN_POINT('Ctrl Pts',(-2.96756453724062,0.866814110013409,
0.599130077738963));
#10445=CARTESIAN_POINT('Ctrl Pts',(-2.90391400488411,-0.0356195898712644,
1.05311670588805));
#10446=CARTESIAN_POINT('Ctrl Pts',(-2.84026347252759,-0.905315579265848,
0.53919129567115));
#10447=CARTESIAN_POINT('Ctrl Pts',(-2.77661294017108,-0.942942489538242,
-0.470300981086807));
#10448=CARTESIAN_POINT('Ctrl Pts',(-2.71296240781457,-0.113917696361458,
-1.04754298711227));
#10449=CARTESIAN_POINT('Ctrl Pts',(-2.64931187545805,0.819808037436047,
-0.661995719884475));
#10450=CARTESIAN_POINT('Ctrl Pts',(-2.58566134310155,1.00005406273575,0.331987082573772));
#10451=CARTESIAN_POINT('Ctrl Pts',(-2.52201081074503,0.261157545803255,
1.0208429299656));
#10452=CARTESIAN_POINT('Ctrl Pts',(-2.45836027838852,-0.717767005130049,
0.771449335819967));
#10453=CARTESIAN_POINT('Ctrl Pts',(-2.39470974603201,-1.03699703112816,
-0.186977829760014));
#10454=CARTESIAN_POINT('Ctrl Pts',(-2.33105921367549,-0.403130496655191,
-0.973555008233726));
#10455=CARTESIAN_POINT('Ctrl Pts',(-2.26740868131899,0.601250396345212,
-0.865344736093925));
#10456=CARTESIAN_POINT('Ctrl Pts',(-2.20375814896247,1.05302634686523,0.0381976988545517));
#10457=CARTESIAN_POINT('Ctrl Pts',(-2.14010761660596,0.536973307373263,
0.906632901762741));
#10458=CARTESIAN_POINT('Ctrl Pts',(-2.07645708424945,-0.472608061478215,
0.941788283861186));
#10459=CARTESIAN_POINT('Ctrl Pts',(-2.01280655189294,-1.04781873848887,
0.111352784695208));
#10460=CARTESIAN_POINT('Ctrl Pts',(-1.94915601953642,-0.659986701133753,
-0.821426263103133));
#10461=CARTESIAN_POINT('Ctrl Pts',(-1.88550548717991,0.334434396684514,
-0.999238302767346));
#10462=CARTESIAN_POINT('Ctrl Pts',(-1.8218549548234,1.02147923051167,-0.258657559338829));
#10463=CARTESIAN_POINT('Ctrl Pts',(-1.75820442246689,0.76968980354421,0.719653498363856));
#10464=CARTESIAN_POINT('Ctrl Pts',(-1.69455389011038,-0.189516021368815,
1.03653616874464));
#10465=CARTESIAN_POINT('Ctrl Pts',(-1.63090335775386,-0.97453902530963,
0.400745853858517));
#10466=CARTESIAN_POINT('Ctrl Pts',(-1.56725282539736,-0.86387017575918,
-0.603367111176601));
#10467=CARTESIAN_POINT('Ctrl Pts',(-1.50360229304084,0.0407755790840783,
-1.05292967668504));
#10468=CARTESIAN_POINT('Ctrl Pts',(-1.43995176068433,0.907944789926865,
-0.534752100240745));
#10469=CARTESIAN_POINT('Ctrl Pts',(-1.37630122832781,0.940628434183195,
0.474912308419707));
#10470=CARTESIAN_POINT('Ctrl Pts',(-1.31265069597131,0.108787204335482,
1.04808821126744));
#10471=CARTESIAN_POINT('Ctrl Pts',(-1.24900016361479,-0.823039563036403,
0.657973723694973));
#10472=CARTESIAN_POINT('Ctrl Pts',(-1.18534963125828,-0.998416558437953,
-0.336879700633251));
#10473=CARTESIAN_POINT('Ctrl Pts',(-1.12169909890177,-0.256156013764477,
-1.0221094195633));
#10474=CARTESIAN_POINT('Ctrl Pts',(-1.05804856654526,0.721535661553076,
-0.767925637542145));
#10475=CARTESIAN_POINT('Ctrl Pts',(-0.994398034188748,1.03606912557217,
0.192053038145565));
#10476=CARTESIAN_POINT('Ctrl Pts',(-0.930747501832232,0.398358748879893,
0.975517275316461));
#10477=CARTESIAN_POINT('Ctrl Pts',(-0.867096969475722,-0.605480095308571,
0.862390297526708));
#10478=CARTESIAN_POINT('Ctrl Pts',(-0.803446437119209,-1.05282691268902,
-0.043352948870463));
#10479=CARTESIAN_POINT('Ctrl Pts',(-0.739795904762697,-0.532527276309977,
-0.909251741039399));
#10480=CARTESIAN_POINT('Ctrl Pts',(-0.676145372406186,0.477212927770878,
-0.939461989031958));
#10481=CARTESIAN_POINT('Ctrl Pts',(-0.612494840049673,1.04835288437428,
-0.106222789101808));
#10482=CARTESIAN_POINT('Ctrl Pts',(-0.548844307693161,0.655953990563453,
0.824651377743634));
#10483=CARTESIAN_POINT('Ctrl Pts',(-0.485193775336649,-0.339317650043208,
0.997582288561571));
#10484=CARTESIAN_POINT('Ctrl Pts',(-0.421543242980137,-1.02274360557363,
0.253665344204375));
#10485=CARTESIAN_POINT('Ctrl Pts',(-0.357892710623625,-0.766137662049351,
-0.723437048700945));
#10486=CARTESIAN_POINT('Ctrl Pts',(-0.294242178267114,0.194552460890076,
-1.03555119121629));
#10487=CARTESIAN_POINT('Ctrl Pts',(-0.230591645910602,0.976558833374166,
-0.396054049992834));
#10488=CARTESIAN_POINT('Ctrl Pts',(-0.166941113554089,0.860773950210724,
0.607750487886167));
#10489=CARTESIAN_POINT('Ctrl Pts',(-0.103290581197577,-0.0456801713590356,
1.05241097889919));
#10490=CARTESIAN_POINT('Ctrl Pts',(-0.0396400488410665,-0.911033846244476,
0.530892604551199));
#10491=CARTESIAN_POINT('Ctrl Pts',(0.0240104835154472,-0.937323228681707,
-0.480729679957274));
#10492=CARTESIAN_POINT('Ctrl Pts',(0.0664441717531208,-0.383082205435835,
-0.857307619105726));
#10493=CARTESIAN_POINT('Ctrl Pts',(0.0876610158719582,-0.0876310866045787,
-0.886512729992231));
#10494=CARTESIAN_POINT('Ctrl Pts',(-4.83325,-0.425119128515126,0.868262223680462));
#10495=CARTESIAN_POINT('Ctrl Pts',(-4.81203315588116,-0.714487838908663,
0.726581322880015));
#10496=CARTESIAN_POINT('Ctrl Pts',(-4.76959946764348,-1.1353522837499,0.133576808423023));
#10497=CARTESIAN_POINT('Ctrl Pts',(-4.70594893528698,-0.725190840417281,
-0.88515665961367));
#10498=CARTESIAN_POINT('Ctrl Pts',(-4.64229840293046,0.352436955761604,
-1.08748877729569));
#10499=CARTESIAN_POINT('Ctrl Pts',(-4.57864787057396,1.10565474053798,-0.291755590264258));
#10500=CARTESIAN_POINT('Ctrl Pts',(-4.51499733821743,0.842928783360187,
0.772877615781201));
#10501=CARTESIAN_POINT('Ctrl Pts',(-4.45134680586093,-0.194661556508119,
1.12677045976561));
#10502=CARTESIAN_POINT('Ctrl Pts',(-4.38769627350441,-1.05326894908993,
0.445264207186226));
#10503=CARTESIAN_POINT('Ctrl Pts',(-4.3240457411479,-0.943861744684315,
-0.64559058936387));
#10504=CARTESIAN_POINT('Ctrl Pts',(-4.26039520879139,0.0330617382951875,
-1.14303003399354));
#10505=CARTESIAN_POINT('Ctrl Pts',(-4.19674467643488,0.979588033886019,
-0.589949130257096));
#10506=CARTESIAN_POINT('Ctrl Pts',(-4.13309414407837,1.02578743895489,0.505365818893066));
#10507=CARTESIAN_POINT('Ctrl Pts',(-4.06944361172186,0.129190056154238,
1.13619421419903));
#10508=CARTESIAN_POINT('Ctrl Pts',(-4.00579307936534,-0.886143464260495,
0.722759076015831));
#10509=CARTESIAN_POINT('Ctrl Pts',(-3.94214254700883,-1.08702966044104,
-0.354961108677097));
#10510=CARTESIAN_POINT('Ctrl Pts',(-3.87849201465232,-0.288834241933398,
-1.10643783919628));
#10511=CARTESIAN_POINT('Ctrl Pts',(-3.8148414822958,0.774826441689782,-0.840996110192966));
#10512=CARTESIAN_POINT('Ctrl Pts',(-3.75119094993929,1.12634979728258,0.19739947687906));
#10513=CARTESIAN_POINT('Ctrl Pts',(-3.68754041758278,0.442653041775359,
1.05436643450591));
#10514=CARTESIAN_POINT('Ctrl Pts',(-3.62388988522627,-0.64788292845573,
0.942272832517326));
#10515=CARTESIAN_POINT('Ctrl Pts',(-3.56023935286976,-1.14295434637101,
-0.0358570462061456));
#10516=CARTESIAN_POINT('Ctrl Pts',(-3.49658882051324,-0.587544583543369,
-0.981030943518769));
#10517=CARTESIAN_POINT('Ctrl Pts',(-3.43293828815673,0.507873202396195,
-1.02454632548698));
#10518=CARTESIAN_POINT('Ctrl Pts',(-3.36928775580022,1.13650836001352,-0.12640849420105));
#10519=CARTESIAN_POINT('Ctrl Pts',(-3.30563722344371,0.720586804608008,
0.887910476855268));
#10520=CARTESIAN_POINT('Ctrl Pts',(-3.2419866910872,-0.357620932582883,
1.08615727607864));
#10521=CARTESIAN_POINT('Ctrl Pts',(-3.17833615873068,-1.10714182672201,
0.286124683940126));
#10522=CARTESIAN_POINT('Ctrl Pts',(-3.11468562637417,-0.839096579851318,
-0.776883059866511));
#10523=CARTESIAN_POINT('Ctrl Pts',(-3.05103509401766,0.200156336903805,
-1.12586313559855));
#10524=CARTESIAN_POINT('Ctrl Pts',(-2.98738456166115,1.05544699487009,-0.440070449159309));
#10525=CARTESIAN_POINT('Ctrl Pts',(-2.92373402930463,0.940683862513151,
0.650187842081352));
#10526=CARTESIAN_POINT('Ctrl Pts',(-2.86008349694813,-0.0386550853224009,
1.14286313423829));
#10527=CARTESIAN_POINT('Ctrl Pts',(-2.79643296459161,-0.982466420492337,
0.585141087098322));
#10528=CARTESIAN_POINT('Ctrl Pts',(-2.7327824322351,-1.02329988972247,-0.510379951504957));
#10529=CARTESIAN_POINT('Ctrl Pts',(-2.66913189987859,-0.123625743263736,
-1.13681442408694));
#10530=CARTESIAN_POINT('Ctrl Pts',(-2.60548136752208,0.8896719403457,-0.718410883665094));
#10531=CARTESIAN_POINT('Ctrl Pts',(-2.54183083516557,1.08527850157133,0.360278965850167));
#10532=CARTESIAN_POINT('Ctrl Pts',(-2.47818030280905,0.283413347882471,
1.10783899256604));
#10533=CARTESIAN_POINT('Ctrl Pts',(-2.41452977045255,-0.778934988448424,
0.837192118320627));
#10534=CARTESIAN_POINT('Ctrl Pts',(-2.35087923809603,-1.12536974350962,
-0.202912048928519));
#10535=CARTESIAN_POINT('Ctrl Pts',(-2.28722870573952,-0.437485209700368,
-1.05652120210659));
#10536=CARTESIAN_POINT('Ctrl Pts',(-2.22357817338301,0.652488853882203,
-0.939089268795666));
#10537=CARTESIAN_POINT('Ctrl Pts',(-2.15992764102649,1.14276507483476,0.0414529003191383));
#10538=CARTESIAN_POINT('Ctrl Pts',(-2.09627710866998,0.582734082211158,
0.9838960049906));
#10539=CARTESIAN_POINT('Ctrl Pts',(-2.03262657631347,-0.512883640898851,
1.02204732283196));
#10540=CARTESIAN_POINT('Ctrl Pts',(-1.96897604395696,-1.13711367494943,
0.120842250257171));
#10541=CARTESIAN_POINT('Ctrl Pts',(-1.90532551160045,-0.716230656674716,
-0.891428070931655));
#10542=CARTESIAN_POINT('Ctrl Pts',(-1.84167497924393,0.362934839657342,
-1.08439322267577));
#10543=CARTESIAN_POINT('Ctrl Pts',(-1.77802444688742,1.1085295185375,-0.280700312992498));
#10544=CARTESIAN_POINT('Ctrl Pts',(-1.71437391453091,0.835282639000601,
0.780982248317964));
#10545=CARTESIAN_POINT('Ctrl Pts',(-1.6507233821744,-0.205666544798836,
1.12486960651137));
#10546=CARTESIAN_POINT('Ctrl Pts',(-1.58707284981788,-1.05758907695201,
0.434897348046092));
#10547=CARTESIAN_POINT('Ctrl Pts',(-1.52342231746138,-0.937489046677483,
-0.654785954795108));
#10548=CARTESIAN_POINT('Ctrl Pts',(-1.45977178510486,0.0442504670677577,
-1.14266016643808));
#10549=CARTESIAN_POINT('Ctrl Pts',(-1.39612125274835,0.985319692043174,
-0.580323584180818));
#10550=CARTESIAN_POINT('Ctrl Pts',(-1.33247072039184,1.02078863095971,0.515384255376705));
#10551=CARTESIAN_POINT('Ctrl Pts',(-1.26882018803533,0.118058031571186,
1.13740611215281));
#10552=CARTESIAN_POINT('Ctrl Pts',(-1.20516965567881,-0.893178856013588,
0.714046133637553));
#10553=CARTESIAN_POINT('Ctrl Pts',(-1.1415191233223,-1.083501449433,-0.365588531996847));
#10554=CARTESIAN_POINT('Ctrl Pts',(-1.07786859096579,-0.277985586125515,
-1.10921341219399));
#10555=CARTESIAN_POINT('Ctrl Pts',(-1.01421805860928,0.783024809137248,
-0.833368131068894));
#10556=CARTESIAN_POINT('Ctrl Pts',(-0.950567526252768,1.12436276199838,
0.208419765718113));
#10557=CARTESIAN_POINT('Ctrl Pts',(-0.886916993896253,0.432306814383134,
1.05865069325971));
#10558=CARTESIAN_POINT('Ctrl Pts',(-0.823266461539743,-0.657079007079016,
0.935883053471222));
#10559=CARTESIAN_POINT('Ctrl Pts',(-0.75961592918323,-1.14254864491163,
-0.0470474798733555));
#10560=CARTESIAN_POINT('Ctrl Pts',(-0.695965396826718,-0.577909161129291,
-0.986738021309451));
#10561=CARTESIAN_POINT('Ctrl Pts',(-0.632314864470206,0.517880933121601,
-1.01952278154909));
#10562=CARTESIAN_POINT('Ctrl Pts',(-0.568664332113694,1.13769334065725,
-0.1152750773031));
#10563=CARTESIAN_POINT('Ctrl Pts',(-0.505013799757181,0.711854279188651,
0.89492802929877));
#10564=CARTESIAN_POINT('Ctrl Pts',(-0.441363267400671,-0.368234243045014,
1.08259608321822));
#10565=CARTESIAN_POINT('Ctrl Pts',(-0.377712735044158,-1.10990164342934,
0.275282662124885));
#10566=CARTESIAN_POINT('Ctrl Pts',(-0.314062202687646,-0.831427784605666,
-0.785088232177701));
#10567=CARTESIAN_POINT('Ctrl Pts',(-0.250411670331134,0.211132188848056,
-1.12380068936391));
#10568=CARTESIAN_POINT('Ctrl Pts',(-0.186761137974623,1.05978101271971,
-0.429805709444989));
#10569=CARTESIAN_POINT('Ctrl Pts',(-0.12311060561811,0.934128961309134,
0.659542882129782));
#10570=CARTESIAN_POINT('Ctrl Pts',(-0.0594600732615982,-0.0495730278705432,
1.14209726531426));
#10571=CARTESIAN_POINT('Ctrl Pts',(0.00419045909491271,-0.98867199722003,
0.576135182918477));
#10572=CARTESIAN_POINT('Ctrl Pts',(0.0678409914514262,-1.01720175640192,
-0.521697382337163));
#10573=CARTESIAN_POINT('Ctrl Pts',(0.1102746796891,-0.415728406479062,-0.93036723005103));
#10574=CARTESIAN_POINT('Ctrl Pts',(0.131491523807937,-0.0950989930495577,
-0.962061195569679));
#10575=CARTESIAN_POINT('',(9.41794719577995E-16,-0.803112203687783,0.541075246555407));
#10576=CARTESIAN_POINT('Ctrl Pts',(-1.94289029309402E-16,-0.803126186815644,
0.541081192037164));
#10577=CARTESIAN_POINT('Ctrl Pts',(-9.19894979498548E-17,-0.812981351345194,
0.522314843079663));
#10578=CARTESIAN_POINT('Ctrl Pts',(1.01398972679205E-15,-0.822159274968141,
0.50322568226441));
#10579=CARTESIAN_POINT('Ctrl Pts',(8.60422844084496E-16,-0.830627172993807,
0.483830163376288));
#10580=CARTESIAN_POINT('Ctrl Pts',(5.866203378691E-16,-0.845771419240517,
0.449142627787863));
#10581=CARTESIAN_POINT('Ctrl Pts',(6.26531303319604E-17,-0.858646531676652,
0.413475093312561));
#10582=CARTESIAN_POINT('Ctrl Pts',(1.2490009027033E-16,-0.869268060390204,
0.377053773207023));
#10583=CARTESIAN_POINT('Ctrl Pts',(1.60510100643605E-16,-0.87534438521063,
0.356217999250341));
#10584=CARTESIAN_POINT('Ctrl Pts',(9.7330067404016E-16,-0.880682551897466,
0.335135479364814));
#10585=CARTESIAN_POINT('Ctrl Pts',(1.02695629777827E-15,-0.885280658259567,
0.313849148426014));
#10586=CARTESIAN_POINT('Ctrl Pts',(1.05599844676046E-15,-0.887769472678274,
0.302327508170255));
#10587=CARTESIAN_POINT('Ctrl Pts',(2.95502323679815E-16,-0.890041495546104,
0.29074449746345));
#10588=CARTESIAN_POINT('Ctrl Pts',(3.46944695195361E-16,-0.892092898041589,
0.27912830849815));
#10589=CARTESIAN_POINT('Ctrl Pts',(5.29096576617445E-16,-0.89935669271314,
0.237996637996833));
#10590=CARTESIAN_POINT('Ctrl Pts',(8.31083498653315E-16,-0.90387239631677,
0.19638846839431));
#10591=CARTESIAN_POINT('Ctrl Pts',(9.15933995315754E-16,-0.905653041946365,
0.154612418313237));
#10592=CARTESIAN_POINT('Ctrl Pts',(9.64512914851158E-16,-0.906672503754648,
0.130694639923923));
#10593=CARTESIAN_POINT('Ctrl Pts',(2.57626188566846E-16,-0.906794503098348,
0.106721941304092));
#10594=CARTESIAN_POINT('Ctrl Pts',(3.88578058618805E-16,-0.906014197420819,
0.0827548331468846));
#10595=CARTESIAN_POINT('Ctrl Pts',(4.3851160086328E-16,-0.905716657366621,
0.0736158830336029));
#10596=CARTESIAN_POINT('Ctrl Pts',(-2.77002943778076E-16,-0.905287870269719,
0.0644777746792196));
#10597=CARTESIAN_POINT('Ctrl Pts',(-4.16333634234434E-16,-0.904727375655016,
0.0553439842300199));
#10598=CARTESIAN_POINT('Ctrl Pts',(-5.42650200061282E-16,-0.904219233804417,
0.0470633316419503));
#10599=CARTESIAN_POINT('Ctrl Pts',(2.51424285193611E-15,-0.903603030759053,
0.0387904666486157));
#10600=CARTESIAN_POINT('Ctrl Pts',(2.48412401759879E-15,-0.90287955572934,
0.0305356644702249));
#10601=CARTESIAN_POINT('Ctrl Pts',(2.33823592373267E-15,-0.899375223793301,
-0.00944853085285923));
#10602=CARTESIAN_POINT('Ctrl Pts',(2.10863171067476E-15,-0.893354572191288,
-0.0490662757321607));
#10603=CARTESIAN_POINT('Ctrl Pts',(1.76247905159244E-15,-0.884825386954599,
-0.0880402565066768));
#10604=CARTESIAN_POINT('Ctrl Pts',(1.42441438509284E-15,-0.876495489474688,
-0.126103594941309));
#10605=CARTESIAN_POINT('Ctrl Pts',(6.30338012388862E-17,-0.865772452890916,
-0.163553884661831));
#10606=CARTESIAN_POINT('Ctrl Pts',(4.85722573273506E-16,-0.85262269549566,
-0.20010706556321));
#10607=CARTESIAN_POINT('Ctrl Pts',(6.80489380870698E-16,-0.846563541721068,
-0.216950064059279));
#10608=CARTESIAN_POINT('Ctrl Pts',(1.48429490985556E-16,-0.839988614098465,
-0.233602136689563));
#10609=CARTESIAN_POINT('Ctrl Pts',(1.66533453693773E-16,-0.83289200456566,
-0.250032742771033));
#10610=CARTESIAN_POINT('Ctrl Pts',(1.75584528646058E-16,-0.82934405510157,
-0.258247223189034));
#10611=CARTESIAN_POINT('Ctrl Pts',(4.14584678018312E-16,-0.825665686482425,
-0.266406317260228));
#10612=CARTESIAN_POINT('Ctrl Pts',(3.7470027081099E-16,-0.821856015550336,
-0.274506010776465));
#10613=CARTESIAN_POINT('Ctrl Pts',(3.43267970675415E-16,-0.81885367131258,
-0.280889257148541));
#10614=CARTESIAN_POINT('Ctrl Pts',(-9.52144087275103E-16,-0.815770670307773,
-0.287233532752809));
#10615=CARTESIAN_POINT('Ctrl Pts',(-9.0205620750794E-16,-0.812610775320565,
-0.293529254379885));
#10616=CARTESIAN_POINT('Ctrl Pts',(-6.42918166058578E-16,-0.796262528958824,
-0.326101225474188));
#10617=CARTESIAN_POINT('Ctrl Pts',(1.17498775833593E-15,-0.777830264118499,
-0.357437379306182));
#10618=CARTESIAN_POINT('Ctrl Pts',(7.7715611723761E-16,-0.757296762434669,
-0.387304251359704));
#10619=CARTESIAN_POINT('Ctrl Pts',(3.9853524207887E-16,-0.73849024909747,
-0.414659143684635));
#10620=CARTESIAN_POINT('Ctrl Pts',(1.27185650954474E-15,-0.717919958048909,
-0.4407813756972));
#10621=CARTESIAN_POINT('Ctrl Pts',(1.65145674912992E-15,-0.695747347291049,
-0.465575322881926));
#10622=CARTESIAN_POINT('Ctrl Pts',(2.0196885785164E-15,-0.674238770187506,
-0.489626731646895));
#10623=CARTESIAN_POINT('Ctrl Pts',(-1.20665404160956E-15,-0.65122178161141,
-0.512428304761557));
#10624=CARTESIAN_POINT('Ctrl Pts',(-1.63757896132211E-15,-0.626835898814702,
-0.533867866368758));
#10625=CARTESIAN_POINT('Ctrl Pts',(-1.74499138019245E-15,-0.620757469516089,
-0.539211895145942));
#10626=CARTESIAN_POINT('Ctrl Pts',(-1.61099258911332E-15,-0.614599937889997,
-0.544465863709149));
#10627=CARTESIAN_POINT('Ctrl Pts',(-1.47798440153224E-15,-0.608370084384792,
-0.549625059375066));
#10628=CARTESIAN_POINT('Ctrl Pts',(-8.64634635312026E-16,-0.579641934182201,
-0.573416011745164));
#10629=CARTESIAN_POINT('Ctrl Pts',(6.37401473877702E-16,-0.549349184522394,
-0.595220439906165));
#10630=CARTESIAN_POINT('Ctrl Pts',(1.11022302462516E-16,-0.517731045324404,
-0.614909901576235));
#10631=CARTESIAN_POINT('Ctrl Pts',(-4.08797301286247E-16,-0.486506921191634,
-0.634353999517735));
#10632=CARTESIAN_POINT('Ctrl Pts',(-8.14248092317691E-16,-0.453988957855334,
-0.651735784095348));
#10633=CARTESIAN_POINT('Ctrl Pts',(-4.30211422042248E-16,-0.420399090453747,
-0.666882017925374));
#10634=CARTESIAN_POINT('Ctrl Pts',(-2.48618918486168E-16,-0.404516054828018,
-0.674043944724363));
#10635=CARTESIAN_POINT('Ctrl Pts',(-1.2985369839148E-15,-0.388393348172599,
-0.680705280104236));
#10636=CARTESIAN_POINT('Ctrl Pts',(-1.35655375821386E-15,-0.372054983150476,
-0.686843528190718));
#10637=CARTESIAN_POINT('Ctrl Pts',(-1.38812292449249E-15,-0.363164648099348,
-0.690183585904075));
#10638=CARTESIAN_POINT('Ctrl Pts',(-1.5894899466084E-15,-0.35420736742959,
-0.693369566369619));
#10639=CARTESIAN_POINT('Ctrl Pts',(-1.40512601554121E-15,-0.34521092676812,
-0.696390075785826));
#10640=CARTESIAN_POINT('Ctrl Pts',(-7.18929174102256E-16,-0.311726453257715,
-0.707632318283803));
#10641=CARTESIAN_POINT('Ctrl Pts',(4.08779474623493E-16,-0.277634746528322,
-0.716612368227301));
#10642=CARTESIAN_POINT('Ctrl Pts',(4.11129463806503E-16,-0.243139933887259,
-0.723191888447147));
#10643=CARTESIAN_POINT('Ctrl Pts',(4.13393983222156E-16,-0.209899707281216,
-0.729532109666564));
#10644=CARTESIAN_POINT('Ctrl Pts',(-6.02471801723509E-16,-0.176284231911036,
-0.733643153360021));
#10645=CARTESIAN_POINT('Ctrl Pts',(-6.08887940067859E-16,-0.142484728679064,
-0.735354534098147));
#10646=CARTESIAN_POINT('Ctrl Pts',(-6.13291820873705E-16,-0.119285574368207,
-0.736529184079122));
#10647=CARTESIAN_POINT('Ctrl Pts',(-3.13452692651376E-17,-0.0959999050278997,
-0.736572366932102));
#10648=CARTESIAN_POINT('Ctrl Pts',(0.,-0.0726952737146206,-0.735415798837336));
#10649=CARTESIAN_POINT('Ctrl Pts',(-0.362235916889675,-0.966647958720147,
0.000894507509818508));
#10650=CARTESIAN_POINT('Ctrl Pts',(-0.346178012155665,-0.964406627548113,
-0.242951400166193));
#10651=CARTESIAN_POINT('Ctrl Pts',(-0.330120107421656,-0.870716846742856,
-0.488329820724893));
#10652=CARTESIAN_POINT('Ctrl Pts',(-0.314062202687646,-0.704080098833991,
-0.664811825991639));
#10653=CARTESIAN_POINT('Ctrl Pts',(-0.292845358568809,-0.483907793454425,
-0.897992384573105));
#10654=CARTESIAN_POINT('Ctrl Pts',(-0.271628514449971,-0.136387802303186,
-1.01089653696851));
#10655=CARTESIAN_POINT('Ctrl Pts',(-0.250411670331134,0.178813663917711,
-0.951682783179724));
#10656=CARTESIAN_POINT('Ctrl Pts',(-0.229194826212297,0.494015130138603,
-0.892469029390939));
#10657=CARTESIAN_POINT('Ctrl Pts',(-0.207977982093461,0.776898071429149,
-0.661137369417972));
#10658=CARTESIAN_POINT('Ctrl Pts',(-0.186761137974624,0.897397533505999,
-0.363913440835694));
#10659=CARTESIAN_POINT('Ctrl Pts',(-0.165544293855786,1.01789699558285,
-0.0666895122534076));
#10660=CARTESIAN_POINT('Ctrl Pts',(-0.144327449736948,0.976012978445995,
0.296426684938188));
#10661=CARTESIAN_POINT('Ctrl Pts',(-0.12311060561811,0.791120638347616,
0.558410514064734));
#10662=CARTESIAN_POINT('Ctrl Pts',(-0.101893761499273,0.606228298249245,
0.82039434319127));
#10663=CARTESIAN_POINT('Ctrl Pts',(-0.0806769173804356,0.278327635189352,
0.981245804252767));
#10664=CARTESIAN_POINT('Ctrl Pts',(-0.059460073261599,-0.0421391912321689,
0.967344521050887));
#10665=CARTESIAN_POINT('Ctrl Pts',(-0.0396400488410658,-0.34150795173535,
0.954358434571918));
#10666=CARTESIAN_POINT('Ctrl Pts',(-0.0198200244205329,-0.634389474522699,
0.78887201096157));
#10667=CARTESIAN_POINT('Ctrl Pts',(5.55111512312578E-16,-0.803126186815652,
0.541081192037152));
#10668=CARTESIAN_POINT('',(-4.83325,-0.42987737795232,-0.601104350279416));
#10669=CARTESIAN_POINT('Ctrl Pts',(-4.83325,-0.430804329183753,-0.601983278585461));
#10670=CARTESIAN_POINT('Ctrl Pts',(-4.83325,-0.445477347946626,-0.594578831837823));
#10671=CARTESIAN_POINT('Ctrl Pts',(-4.83325,-0.459859229529849,-0.586662521041488));
#10672=CARTESIAN_POINT('Ctrl Pts',(-4.83325,-0.473920354446851,-0.578240804726048));
#10673=CARTESIAN_POINT('Ctrl Pts',(-4.83325,-0.502699198697331,-0.56100411394957));
#10674=CARTESIAN_POINT('Ctrl Pts',(-4.83325,-0.530135414509647,-0.541653667307754));
#10675=CARTESIAN_POINT('Ctrl Pts',(-4.83325,-0.556162906488769,-0.520445389256222));
#10676=CARTESIAN_POINT('Ctrl Pts',(-4.83325,-0.56908364730694,-0.509917034694693));
#10677=CARTESIAN_POINT('Ctrl Pts',(-4.83325,-0.581657058686961,-0.498930055622465));
#10678=CARTESIAN_POINT('Ctrl Pts',(-4.83325,-0.593873683444419,-0.487511537377947));
#10679=CARTESIAN_POINT('Ctrl Pts',(-4.83325,-0.600533437529337,-0.48128686198418));
#10680=CARTESIAN_POINT('Ctrl Pts',(-4.83325,-0.607080659136859,-0.474939906075632));
#10681=CARTESIAN_POINT('Ctrl Pts',(-4.83325,-0.613511965498124,-0.468477976156228));
#10682=CARTESIAN_POINT('Ctrl Pts',(-4.83325,-0.638749297301084,-0.443120473294029));
#10683=CARTESIAN_POINT('Ctrl Pts',(-4.83325,-0.66221430844257,-0.415986042558697));
#10684=CARTESIAN_POINT('Ctrl Pts',(-4.83325,-0.683827784278158,-0.387356210034121));
#10685=CARTESIAN_POINT('Ctrl Pts',(-4.83325,-0.692968365694583,-0.375248332656129));
#10686=CARTESIAN_POINT('Ctrl Pts',(-4.83325,-0.701777560219736,-0.362872376885599));
#10687=CARTESIAN_POINT('Ctrl Pts',(-4.83325,-0.710248135732303,-0.350247157922094));
#10688=CARTESIAN_POINT('Ctrl Pts',(-4.83325,-0.715937842738501,-0.341766766396764));
#10689=CARTESIAN_POINT('Ctrl Pts',(-4.83325,-0.721474753491652,-0.333173882455301));
#10690=CARTESIAN_POINT('Ctrl Pts',(-4.83325,-0.726856437266772,-0.32447389474923));
#10691=CARTESIAN_POINT('Ctrl Pts',(-4.83325,-0.731149308711402,-0.317534072501648));
#10692=CARTESIAN_POINT('Ctrl Pts',(-4.83325,-0.735338466732717,-0.310534061700282));
#10693=CARTESIAN_POINT('Ctrl Pts',(-4.83325,-0.739422758184052,-0.303477889367202));
#10694=CARTESIAN_POINT('Ctrl Pts',(-4.83325,-0.758372787573866,-0.270739120676307));
#10695=CARTESIAN_POINT('Ctrl Pts',(-4.83325,-0.77507052557327,-0.236790214473258));
#10696=CARTESIAN_POINT('Ctrl Pts',(-4.83325,-0.789429989028317,-0.201931384422613));
#10697=CARTESIAN_POINT('Ctrl Pts',(-4.83325,-0.803883329607414,-0.166844659595597));
#10698=CARTESIAN_POINT('Ctrl Pts',(-4.83325,-0.815968620008672,-0.130835015658004));
#10699=CARTESIAN_POINT('Ctrl Pts',(-4.83325,-0.825564034353866,-0.0941680070552365));
#10700=CARTESIAN_POINT('Ctrl Pts',(-4.83325,-0.830500900753741,-0.0753027328479168));
#10701=CARTESIAN_POINT('Ctrl Pts',(-4.83325,-0.834778029329683,-0.0562628870236651));
#10702=CARTESIAN_POINT('Ctrl Pts',(-4.83325,-0.83837413332027,-0.0370819396298865));
#10703=CARTESIAN_POINT('Ctrl Pts',(-4.83325,-0.839809771420891,-0.0294245139946491));
#10704=CARTESIAN_POINT('Ctrl Pts',(-4.83325,-0.841136658874383,-0.021744760562141));
#10705=CARTESIAN_POINT('Ctrl Pts',(-4.83325,-0.84235147577949,-0.0140588668413698));
#10706=CARTESIAN_POINT('Ctrl Pts',(-4.83325,-0.848299998911048,0.0235762009556639));
#10707=CARTESIAN_POINT('Ctrl Pts',(-4.83325,-0.851580615949718,0.0614395817607659));
#10708=CARTESIAN_POINT('Ctrl Pts',(-4.83325,-0.852097207338896,0.0992623517965642));
#10709=CARTESIAN_POINT('Ctrl Pts',(-4.83325,-0.852615113851108,0.137181409918323));
#10710=CARTESIAN_POINT('Ctrl Pts',(-4.83325,-0.850356236583576,0.175060804309161));
#10711=CARTESIAN_POINT('Ctrl Pts',(-4.83325,-0.845501835307578,0.212700460935093));
#10712=CARTESIAN_POINT('Ctrl Pts',(-4.83325,-0.843195953076148,0.230579620583479));
#10713=CARTESIAN_POINT('Ctrl Pts',(-4.83325,-0.840303662427911,0.248404883782479));
#10714=CARTESIAN_POINT('Ctrl Pts',(-4.83325,-0.836840327249148,0.266155401711081));
#10715=CARTESIAN_POINT('Ctrl Pts',(-4.83325,-0.834753511787874,0.276850888387093));
#10716=CARTESIAN_POINT('Ctrl Pts',(-4.83325,-0.832459323189004,0.287519241621333));
#10717=CARTESIAN_POINT('Ctrl Pts',(-4.83325,-0.829960684482013,0.298155892677309));
#10718=CARTESIAN_POINT('Ctrl Pts',(-4.83325,-0.828117127511462,0.306003874917678));
#10719=CARTESIAN_POINT('Ctrl Pts',(-4.83325,-0.826164420153568,0.313825330995023));
#10720=CARTESIAN_POINT('Ctrl Pts',(-4.83325,-0.824105062345242,0.321616309397643));
#10721=CARTESIAN_POINT('Ctrl Pts',(-4.83325,-0.813982847369566,0.359910751453001));
#10722=CARTESIAN_POINT('Ctrl Pts',(-4.83325,-0.801284425310483,0.397484364452202));
#10723=CARTESIAN_POINT('Ctrl Pts',(-4.83325,-0.786216397836987,0.434122372205131));
#10724=CARTESIAN_POINT('Ctrl Pts',(-4.83325,-0.770800032786528,0.471607365063968));
#10725=CARTESIAN_POINT('Ctrl Pts',(-4.83325,-0.752903064000475,0.508114087518576));
#10726=CARTESIAN_POINT('Ctrl Pts',(-4.83325,-0.732692327044247,0.543415099892429));
#10727=CARTESIAN_POINT('Ctrl Pts',(-4.83325,-0.722980854333143,0.560377609428103));
#10728=CARTESIAN_POINT('Ctrl Pts',(-4.83325,-0.712734375992085,0.577061665953607));
#10729=CARTESIAN_POINT('Ctrl Pts',(-4.83325,-0.701967293126427,0.593441055574146));
#10730=CARTESIAN_POINT('Ctrl Pts',(-4.83325,-0.697220911880786,0.600661472532015));
#10731=CARTESIAN_POINT('Ctrl Pts',(-4.83325,-0.692373330886061,0.607822672059881));
#10732=CARTESIAN_POINT('Ctrl Pts',(-4.83325,-0.687425630630908,0.614922336492617));
#10733=CARTESIAN_POINT('Ctrl Pts',(-4.83325,-0.682711871397128,0.621686309055766));
#10734=CARTESIAN_POINT('Ctrl Pts',(-4.83325,-0.677912762676946,0.628386468272317));
#10735=CARTESIAN_POINT('Ctrl Pts',(-4.83325,-0.673030972331822,0.635019657522898));
#10736=CARTESIAN_POINT('Ctrl Pts',(-4.83325,-0.64794630581489,0.669103739085453));
#10737=CARTESIAN_POINT('Ctrl Pts',(-4.83325,-0.620674189974278,0.701432488552139));
#10738=CARTESIAN_POINT('Ctrl Pts',(-4.83325,-0.591409628166749,0.731768993635442));
#10739=CARTESIAN_POINT('Ctrl Pts',(-4.83325,-0.562348522484787,0.761894590117822));
#10740=CARTESIAN_POINT('Ctrl Pts',(-4.83325,-0.531322040415095,0.790056726268309));
#10741=CARTESIAN_POINT('Ctrl Pts',(-4.83325,-0.498473806854146,0.816006607343616));
#10742=CARTESIAN_POINT('Ctrl Pts',(-4.83325,-0.474944626301769,0.834594499931528));
#10743=CARTESIAN_POINT('Ctrl Pts',(-4.83325,-0.450479728398504,0.852047023038678));
#10744=CARTESIAN_POINT('Ctrl Pts',(-4.83325,-0.425119128515126,0.868262223680462));
#10745=CARTESIAN_POINT('Ctrl Pts',(-4.83325,-0.430804329183755,-0.60198327858546));
#10746=CARTESIAN_POINT('Ctrl Pts',(-4.81342997557947,-0.243786711209356,
-0.73442123871231));
#10747=CARTESIAN_POINT('Ctrl Pts',(-4.77239310704009,0.282044155337814,
-0.817946147254488));
#10748=CARTESIAN_POINT('Ctrl Pts',(-4.71013939438189,0.845181125686649,
-0.223022892376799));
#10749=CARTESIAN_POINT('Ctrl Pts',(-4.64648886202537,0.644348974298595,
0.590800680695443));
#10750=CARTESIAN_POINT('Ctrl Pts',(-4.58283832966888,-0.148802575908472,
0.861322337488271));
#10751=CARTESIAN_POINT('Ctrl Pts',(-4.53191785589294,-0.673870243765561,
0.444558049452164));
#10752=CARTESIAN_POINT('Ctrl Pts',(-4.50221422623585,-0.73843669443239,
0.0992268317336678));
#10753=CARTESIAN_POINT('Ctrl Pts',(-4.49372744069761,-0.73797111367679,
0.000392387352095092));
#10754=CARTESIAN_POINT('Origin',(-4.83325,-2.39206768658147E-16,-5.43753587379397E-17));
#10755=CARTESIAN_POINT('',(-4.83325,-0.96675,-1.1839272930757E-16));
#10756=CARTESIAN_POINT('Origin',(-4.83325,0.,0.));
#10757=CARTESIAN_POINT('Origin',(-4.83325,0.,0.));
#10758=CARTESIAN_POINT('',(-4.83325,0.429877377952362,-0.601104350279386));
#10759=CARTESIAN_POINT('Ctrl Pts',(-4.83325,0.42612583279255,0.869596007169462));
#10760=CARTESIAN_POINT('Ctrl Pts',(-4.83325,0.444028989667205,0.858248011186931));
#10761=CARTESIAN_POINT('Ctrl Pts',(-4.83325,0.461506235194407,0.846282389466895));
#10762=CARTESIAN_POINT('Ctrl Pts',(-4.83325,0.478520947266387,0.833697047115898));
#10763=CARTESIAN_POINT('Ctrl Pts',(-4.83325,0.508950575570106,0.811189038270626));
#10764=CARTESIAN_POINT('Ctrl Pts',(-4.83325,0.537902478796165,0.786699694802319));
#10765=CARTESIAN_POINT('Ctrl Pts',(-4.83325,0.565277284351656,0.76043282750384));
#10766=CARTESIAN_POINT('Ctrl Pts',(-4.83325,0.580937763781647,0.745406173371658));
#10767=CARTESIAN_POINT('Ctrl Pts',(-4.83325,0.596081589422928,0.729797428444441));
#10768=CARTESIAN_POINT('Ctrl Pts',(-4.83325,0.610685694034066,0.71364285438593));
#10769=CARTESIAN_POINT('Ctrl Pts',(-4.83325,0.618590448550963,0.704898878246498));
#10770=CARTESIAN_POINT('Ctrl Pts',(-4.83325,0.626337929842749,0.695993563897982));
#10771=CARTESIAN_POINT('Ctrl Pts',(-4.83325,0.633910755450761,0.68694943481743));
#10772=CARTESIAN_POINT('Ctrl Pts',(-4.83325,0.660725313294558,0.654925150233266));
#10773=CARTESIAN_POINT('Ctrl Pts',(-4.83325,0.685395865650988,0.621116966784517));
#10774=CARTESIAN_POINT('Ctrl Pts',(-4.83325,0.707779749462567,0.585798858308791));
#10775=CARTESIAN_POINT('Ctrl Pts',(-4.83325,0.720595052618967,0.565578405467051));
#10776=CARTESIAN_POINT('Ctrl Pts',(-4.83325,0.732659941452485,0.544862641244956));
#10777=CARTESIAN_POINT('Ctrl Pts',(-4.83325,0.743940032444047,0.523701592965213));
#10778=CARTESIAN_POINT('Ctrl Pts',(-4.83325,0.748241276114926,0.515632613286725));
#10779=CARTESIAN_POINT('Ctrl Pts',(-4.83325,0.752428350379102,0.507498888240225));
#10780=CARTESIAN_POINT('Ctrl Pts',(-4.83325,0.756499122018279,0.499303200814814));
#10781=CARTESIAN_POINT('Ctrl Pts',(-4.83325,0.760189669440217,0.491873019075367));
#10782=CARTESIAN_POINT('Ctrl Pts',(-4.83325,0.763782676895556,0.484395678421437));
#10783=CARTESIAN_POINT('Ctrl Pts',(-4.83325,0.767273702449937,0.476880477828687));
#10784=CARTESIAN_POINT('Ctrl Pts',(-4.83325,0.784183308647347,0.440478830078366));
#10785=CARTESIAN_POINT('Ctrl Pts',(-4.83325,0.798729262844989,0.403139470529216));
#10786=CARTESIAN_POINT('Ctrl Pts',(-4.83325,0.810779971273345,0.365106624276173));
#10787=CARTESIAN_POINT('Ctrl Pts',(-4.83325,0.822549112237606,0.327962423876228));
#10788=CARTESIAN_POINT('Ctrl Pts',(-4.83325,0.83193833949342,0.290155682630556));
#10789=CARTESIAN_POINT('Ctrl Pts',(-4.83325,0.838776841007867,0.251915835838885));
#10790=CARTESIAN_POINT('Ctrl Pts',(-4.83325,0.841927890733968,0.234295651284645));
#10791=CARTESIAN_POINT('Ctrl Pts',(-4.83325,0.844536683340313,0.216583635587054));
#10792=CARTESIAN_POINT('Ctrl Pts',(-4.83325,0.846582862757641,0.198803310308648));
#10793=CARTESIAN_POINT('Ctrl Pts',(-4.83325,0.847605879593024,0.189913780903579));
#10794=CARTESIAN_POINT('Ctrl Pts',(-4.83325,0.848488226313175,0.181007190858287));
#10795=CARTESIAN_POINT('Ctrl Pts',(-4.83325,0.849227134713394,0.172086578880304));
#10796=CARTESIAN_POINT('Ctrl Pts',(-4.83325,0.849809455873283,0.165056396096608));
#10797=CARTESIAN_POINT('Ctrl Pts',(-4.83325,0.850302427402192,0.158019752367885));
#10798=CARTESIAN_POINT('Ctrl Pts',(-4.83325,0.850704529741687,0.150986829435613));
#10799=CARTESIAN_POINT('Ctrl Pts',(-4.83325,0.852784787481737,0.114602329948682));
#10800=CARTESIAN_POINT('Ctrl Pts',(-4.83325,0.852442432887478,0.0782492400763008));
#10801=CARTESIAN_POINT('Ctrl Pts',(-4.83325,0.849546081607686,0.0421212997055655));
#10802=CARTESIAN_POINT('Ctrl Pts',(-4.83325,0.846893292297877,0.00903145502076376));
#10803=CARTESIAN_POINT('Ctrl Pts',(-4.83325,0.842096943578794,-0.023869961011144));
#10804=CARTESIAN_POINT('Ctrl Pts',(-4.83325,0.835249263413218,-0.0564195258552621));
#10805=CARTESIAN_POINT('Ctrl Pts',(-4.83325,0.828606660361437,-0.0879942830780913));
#10806=CARTESIAN_POINT('Ctrl Pts',(-4.83325,0.820033249827154,-0.11923833161495));
#10807=CARTESIAN_POINT('Ctrl Pts',(-4.83325,0.809593987319783,-0.149984849812598));
#10808=CARTESIAN_POINT('Ctrl Pts',(-4.83325,0.806991894894374,-0.157648732395617));
#10809=CARTESIAN_POINT('Ctrl Pts',(-4.83325,0.804276318225724,-0.165274023246567));
#10810=CARTESIAN_POINT('Ctrl Pts',(-4.83325,0.801450782783496,-0.172853255423677));
#10811=CARTESIAN_POINT('Ctrl Pts',(-4.83325,0.78842119754443,-0.207803888221425));
#10812=CARTESIAN_POINT('Ctrl Pts',(-4.83325,0.77304459857233,-0.241813369413132));
#10813=CARTESIAN_POINT('Ctrl Pts',(-4.83325,0.755464227887144,-0.274651045788919));
#10814=CARTESIAN_POINT('Ctrl Pts',(-4.83325,0.738102943775821,-0.307079499052199));
#10815=CARTESIAN_POINT('Ctrl Pts',(-4.83325,0.718591500210376,-0.338366042204787));
#10816=CARTESIAN_POINT('Ctrl Pts',(-4.83325,0.697035820681698,-0.368249817141349));
#10817=CARTESIAN_POINT('Ctrl Pts',(-4.83325,0.686843175319872,-0.382380418758235));
#10818=CARTESIAN_POINT('Ctrl Pts',(-4.83325,0.676193084355949,-0.396196732108217));
#10819=CARTESIAN_POINT('Ctrl Pts',(-4.83325,0.66509513654706,-0.409667281285853));
#10820=CARTESIAN_POINT('Ctrl Pts',(-4.83325,0.659056302451551,-0.416997142000641));
#10821=CARTESIAN_POINT('Ctrl Pts',(-4.83325,0.652882583585388,-0.424226863698243));
#10822=CARTESIAN_POINT('Ctrl Pts',(-4.83325,0.646592377244359,-0.431332710172516));
#10823=CARTESIAN_POINT('Ctrl Pts',(-4.83325,0.623180471355048,-0.457780397243514));
#10824=CARTESIAN_POINT('Ctrl Pts',(-4.83325,0.598113758680377,-0.482570416996733));
#10825=CARTESIAN_POINT('Ctrl Pts',(-4.83325,0.571500139611121,-0.505481042427813));
#10826=CARTESIAN_POINT('Ctrl Pts',(-4.83325,0.545854470535468,-0.527558397506533));
#10827=CARTESIAN_POINT('Ctrl Pts',(-4.83325,0.518771520661077,-0.547890969440507));
#10828=CARTESIAN_POINT('Ctrl Pts',(-4.83325,0.490331967004018,-0.566235607805961));
#10829=CARTESIAN_POINT('Ctrl Pts',(-4.83325,0.470811710682197,-0.57882694617023));
#10830=CARTESIAN_POINT('Ctrl Pts',(-4.83325,0.450652020252665,-0.590480820623256));
#10831=CARTESIAN_POINT('Ctrl Pts',(-4.83325,0.429877377952375,-0.601104350279377));
#10832=CARTESIAN_POINT('Origin',(-4.83325,0.,0.));
#10833=CARTESIAN_POINT('Origin',(-5.57277255930238,0.,0.));
#10834=CARTESIAN_POINT('Ctrl Pts',(-4.83325,0.429877377952362,-0.601104350279386));
#10835=CARTESIAN_POINT('Ctrl Pts',(-4.81203315588116,0.630209473381985,
-0.457837651472495));
#10836=CARTESIAN_POINT('Ctrl Pts',(-4.76959946764349,0.872845016829865,
0.0422750560198467));
#10837=CARTESIAN_POINT('Ctrl Pts',(-4.70594893528698,0.435295217673284,
0.758713395217541));
#10838=CARTESIAN_POINT('Ctrl Pts',(-4.64229840293046,-0.402686892608664,
0.775548661280791));
#10839=CARTESIAN_POINT('Ctrl Pts',(-4.59790627760226,-0.728869356585195,
0.290955964823503));
#10840=CARTESIAN_POINT('Ctrl Pts',(-4.5747309963929,-0.740099763884578,
0.0230972773004798));
#10841=CARTESIAN_POINT('Ctrl Pts',(-4.57277255930238,-0.73995294767526,
0.000448391410152972));
#10842=CARTESIAN_POINT('Ctrl Pts',(-4.96474152380794,0.56235988516297,-0.786356739692293));
#10843=CARTESIAN_POINT('Ctrl Pts',(-4.9435246796891,0.824431675767287,-0.598937144196273));
#10844=CARTESIAN_POINT('Ctrl Pts',(-4.90109099145142,1.14184427607615,0.0553036676687026));
#10845=CARTESIAN_POINT('Ctrl Pts',(-4.83744045909491,0.569447431239055,
0.992538802201013));
#10846=CARTESIAN_POINT('Ctrl Pts',(-4.7737899267384,-0.526789652813818,
1.01456247400976));
#10847=CARTESIAN_POINT('Ctrl Pts',(-4.71013939438189,-1.13861357503166,
0.105606791321867));
#10848=CARTESIAN_POINT('Ctrl Pts',(-4.64648886202538,-0.70407473659118,
-0.901192246508667));
#10849=CARTESIAN_POINT('Ctrl Pts',(-4.58283832966887,0.377642053273196,
-1.07930139350315));
#10850=CARTESIAN_POINT('Ctrl Pts',(-4.51918779731235,1.11223495243478,-0.265648574991642));
#10851=CARTESIAN_POINT('Ctrl Pts',(-4.45553726495584,0.824599510160386,
0.792273888950893));
#10852=CARTESIAN_POINT('Ctrl Pts',(-4.39188673259932,-0.220929385279549,
1.12196304044685));
#10853=CARTESIAN_POINT('Ctrl Pts',(-4.32823620024282,-1.06339842520545,
0.420495621507773));
#10854=CARTESIAN_POINT('Ctrl Pts',(-4.2645856678863,-0.928508331559392,
-0.66746299315913));
#10855=CARTESIAN_POINT('Ctrl Pts',(-4.20093513552979,0.0597685883364044,
-1.14195235318934));
#10856=CARTESIAN_POINT('Ctrl Pts',(-4.13728460317328,0.99311185945035,-0.566886097296187));
#10857=CARTESIAN_POINT('Ctrl Pts',(-4.07363407081677,1.01369352163242,0.529203559900727));
#10858=CARTESIAN_POINT('Ctrl Pts',(-4.00998353846026,0.102596499545881,
1.13890472099335));
#10859=CARTESIAN_POINT('Ctrl Pts',(-3.94633300610375,-0.902796119909644,
0.701847369912606));
#10860=CARTESIAN_POINT('Ctrl Pts',(-3.88268247374723,-1.0784353364453,-0.380273240325727));
#10861=CARTESIAN_POINT('Ctrl Pts',(-3.81903194139072,-0.262892311079046,
-1.11288724474915));
#10862=CARTESIAN_POINT('Ctrl Pts',(-3.75538140903421,0.794273142239551,
-0.822654634904011));
#10863=CARTESIAN_POINT('Ctrl Pts',(-3.69173087667769,1.1214278354034,0.223674023103978));
#10864=CARTESIAN_POINT('Ctrl Pts',(-3.62808034432119,0.417886214707462,
1.0644254574015));
#10865=CARTESIAN_POINT('Ctrl Pts',(-3.56442981196467,-0.669731637124126,
0.926871075173695));
#10866=CARTESIAN_POINT('Ctrl Pts',(-3.50077927960816,-1.14180392873907,
-0.0625638960671715));
#10867=CARTESIAN_POINT('Ctrl Pts',(-3.43712874725165,-0.56445238861775,
-0.994496833509968));
#10868=CARTESIAN_POINT('Ctrl Pts',(-3.37347821489514,0.531683307704501,
-1.01239484051207));
#10869=CARTESIAN_POINT('Ctrl Pts',(-3.30982768253862,1.13915267574454,-0.0998079835003414));
#10870=CARTESIAN_POINT('Ctrl Pts',(-3.24617715018212,0.699634960298149,
0.904511677284527));
#10871=CARTESIAN_POINT('Ctrl Pts',(-3.1825266178256,-0.382912247206447,
1.07750111982801));
#10872=CARTESIAN_POINT('Ctrl Pts',(-3.11887608546909,-1.11352754479072,
0.260166983272478));
#10873=CARTESIAN_POINT('Ctrl Pts',(-3.05522555311258,-0.82070763370308,
-0.796284768254284));
#10874=CARTESIAN_POINT('Ctrl Pts',(-2.99157502075606,0.226418798374384,
-1.12087687992661));
#10875=CARTESIAN_POINT('Ctrl Pts',(-2.92792448839955,1.06544533095863,-0.415279061515531));
#10876=CARTESIAN_POINT('Ctrl Pts',(-2.86427395604304,0.925228673999507,
0.671998774554289));
#10877=CARTESIAN_POINT('Ctrl Pts',(-2.80062342368653,-0.0653590451388047,
1.14164733933789));
#10878=CARTESIAN_POINT('Ctrl Pts',(-2.73697289133001,-0.995875732975225,
0.562015993248534));
#10879=CARTESIAN_POINT('Ctrl Pts',(-2.67332235897351,-1.01109015160153,
-0.534160235819258));
#10880=CARTESIAN_POINT('Ctrl Pts',(-2.60967182661699,-0.0970188375877351,
-1.13939360949144));
#10881=CARTESIAN_POINT('Ctrl Pts',(-2.54602129426048,0.906221796713611,
-0.697418459289406));
#10882=CARTESIAN_POINT('Ctrl Pts',(-2.48237076190397,1.07656045391649,0.385549012785039));
#10883=CARTESIAN_POINT('Ctrl Pts',(-2.41872022954745,0.25744009150123,1.11416114251229));
#10884=CARTESIAN_POINT('Ctrl Pts',(-2.35506969719094,-0.798291619232457,
0.818755728444102));
#10885=CARTESIAN_POINT('Ctrl Pts',(-2.29141916483443,-1.12031920767361,
-0.229162224447393));
#10886=CARTESIAN_POINT('Ctrl Pts',(-2.22776863247792,-0.41266941863844,
-1.06645881454311));
#10887=CARTESIAN_POINT('Ctrl Pts',(-2.16411810012141,0.674261883950841,
-0.923580729579072));
#10888=CARTESIAN_POINT('Ctrl Pts',(-2.1004675677649,1.14148390757138,0.0681538036277071));
#10889=CARTESIAN_POINT('Ctrl Pts',(-2.03681703540839,0.559576229296189,
0.997248662972996));
#10890=CARTESIAN_POINT('Ctrl Pts',(-1.97316650305187,-0.536633962355949,
1.00977940296753));
#10891=CARTESIAN_POINT('Ctrl Pts',(-1.90951597069536,-1.13962771421169,
0.0942291100080961));
#10892=CARTESIAN_POINT('Ctrl Pts',(-1.84586543833885,-0.695197778253047,
-0.907926484526569));
#10893=CARTESIAN_POINT('Ctrl Pts',(-1.78221490598234,0.388183467573543,
-1.07561333563409));
#10894=CARTESIAN_POINT('Ctrl Pts',(-1.71856437362583,1.11478806235877,-0.254711656658762));
#10895=CARTESIAN_POINT('Ctrl Pts',(-1.65491384126931,0.816798916034974,
0.800293685462062));
#10896=CARTESIAN_POINT('Ctrl Pts',(-1.5912633089128,-0.231904277260913,
1.1197548209207));
#10897=CARTESIAN_POINT('Ctrl Pts',(-1.52761277655629,-1.06746590576262,
0.410057301985987));
#10898=CARTESIAN_POINT('Ctrl Pts',(-1.46396224419978,-0.921927250481219,
-0.676520951335004));
#10899=CARTESIAN_POINT('Ctrl Pts',(-1.40031171184326,0.0709481552934287,
-1.14131363569313));
#10900=CARTESIAN_POINT('Ctrl Pts',(-1.33666117948675,0.99861561272938,-0.557133108709257));
#10901=CARTESIAN_POINT('Ctrl Pts',(-1.27301064713024,1.00846260812683,0.539104467278014));
#10902=CARTESIAN_POINT('Ctrl Pts',(-1.20936011477373,0.091438806302383,
1.13985499845995));
#10903=CARTESIAN_POINT('Ctrl Pts',(-1.14570958241722,-0.909625709061619,
0.6929729115658));
#10904=CARTESIAN_POINT('Ctrl Pts',(-1.0820590500607,-1.07465981147156,-0.390815559835605));
#10905=CARTESIAN_POINT('Ctrl Pts',(-1.01840851770419,-0.25198161758667,
-1.11540836879394));
#10906=CARTESIAN_POINT('Ctrl Pts',(-0.95475798534768,0.802290807826833,
-0.814837078744325));
#10907=CARTESIAN_POINT('Ctrl Pts',(-0.891107452991169,1.11918400223162,
0.234644694719414));
#10908=CARTESIAN_POINT('Ctrl Pts',(-0.827456920634655,0.407442197441156,
1.06846706473946));
#10909=CARTESIAN_POINT('Ctrl Pts',(-0.763806388278144,-0.678774957884412,
0.920267362050519));
#10910=CARTESIAN_POINT('Ctrl Pts',(-0.700155855921631,-1.14113843231311,
-0.0737404048682484));
#10911=CARTESIAN_POINT('Ctrl Pts',(-0.636505323565119,-0.554683026357975,
-0.999979759148649));
#10912=CARTESIAN_POINT('Ctrl Pts',(-0.572854791208608,0.541564867027828,
-1.00713373104562));
#10913=CARTESIAN_POINT('Ctrl Pts',(-0.509204258852095,1.14008849478539,
-0.088659411954491));
#10914=CARTESIAN_POINT('Ctrl Pts',(-0.445553726495583,0.690719139687767,
0.9113412230782));
#10915=CARTESIAN_POINT('Ctrl Pts',(-0.381903194139072,-0.393398339859427,
1.0736585884787));
#10916=CARTESIAN_POINT('Ctrl Pts',(-0.318252661782559,-1.11611113297518,
0.249328375284737));
#10917=CARTESIAN_POINT('Ctrl Pts',(-0.254602129426048,-0.812701078288131,
-0.804431864715086));
#10918=CARTESIAN_POINT('Ctrl Pts',(-0.190951597069537,0.237061432483635,
-1.11832295389539));
#10919=CARTESIAN_POINT('Ctrl Pts',(-0.127301064713023,1.07008226849263,
-0.40537339512733));
#10920=CARTESIAN_POINT('Ctrl Pts',(-0.0636505323565116,0.917349355006781,
0.682156145859666));
#10921=CARTESIAN_POINT('Ctrl Pts',(-0.0212168441188374,0.256765040167821,
0.986146543295702));
#10922=CARTESIAN_POINT('Ctrl Pts',(0.,-0.0647045675182444,0.964582231560522));
#10923=CARTESIAN_POINT('Ctrl Pts',(-4.92091101587196,0.5181990494261,-0.724605943221324));
#10924=CARTESIAN_POINT('Ctrl Pts',(-4.89969417175312,0.759690941638853,
-0.551903979955014));
#10925=CARTESIAN_POINT('Ctrl Pts',(-4.85726048351545,1.05217785632739,0.0509607971190845));
#10926=CARTESIAN_POINT('Ctrl Pts',(-4.79360995115893,0.524730026717131,
0.914596999873189));
#10927=CARTESIAN_POINT('Ctrl Pts',(-4.72995941880242,-0.485422066078767,
0.934891203100105));
#10928=CARTESIAN_POINT('Ctrl Pts',(-4.66630888644591,-1.04920085484773,
0.0973137315085493));
#10929=CARTESIAN_POINT('Ctrl Pts',(-4.60265835408939,-0.648785357655345,
-0.830423680301498));
#10930=CARTESIAN_POINT('Ctrl Pts',(-4.53900782173289,0.347986686448627,
-0.994546323295287));
#10931=CARTESIAN_POINT('Ctrl Pts',(-4.47535728937637,1.02489368515885,-0.244787799901783));
#10932=CARTESIAN_POINT('Ctrl Pts',(-4.41170675701986,0.759845596380872,
0.730058432280414));
#10933=CARTESIAN_POINT('Ctrl Pts',(-4.34805622466335,-0.203580305890738,
1.03385784866622));
#10934=CARTESIAN_POINT('Ctrl Pts',(-4.28440569230684,-0.979892178729958,
0.387475061970349));
#10935=CARTESIAN_POINT('Ctrl Pts',(-4.22075515995032,-0.85559469566157,
-0.615048650708658));
#10936=CARTESIAN_POINT('Ctrl Pts',(-4.15710462759381,0.0550750977774527,
-1.05227744639204));
#10937=CARTESIAN_POINT('Ctrl Pts',(-4.0934540952373,0.915125056247244,-0.522369828471353));
#10938=CARTESIAN_POINT('Ctrl Pts',(-4.02980356288079,0.934090487565776,
0.487646414562436));
#10939=CARTESIAN_POINT('Ctrl Pts',(-3.96615303052428,0.0945398310615815,
1.04946913778286));
#10940=CARTESIAN_POINT('Ctrl Pts',(-3.90250249816776,-0.83190160519215,
0.646732900988337));
#10941=CARTESIAN_POINT('Ctrl Pts',(-3.83885196581125,-0.993748275717631,
-0.350411252399111));
#10942=CARTESIAN_POINT('Ctrl Pts',(-3.77520143345474,-0.242247979091021,
-1.02549475444948));
#10943=CARTESIAN_POINT('Ctrl Pts',(-3.71155090109823,0.731900688780351,
-0.758053447730699));
#10944=CARTESIAN_POINT('Ctrl Pts',(-3.64790036874172,1.03336467205089,0.20610941358345));
#10945=CARTESIAN_POINT('Ctrl Pts',(-3.58424983638521,0.38507056591869,0.980838560436342));
#10946=CARTESIAN_POINT('Ctrl Pts',(-3.52059930402869,-0.617139143251182,
0.854086009275647));
#10947=CARTESIAN_POINT('Ctrl Pts',(-3.45694877167218,-1.05214067737442,
-0.0576508963846335));
#10948=CARTESIAN_POINT('Ctrl Pts',(-3.39329823931567,-0.520127233369855,
-0.916401271461218));
#10949=CARTESIAN_POINT('Ctrl Pts',(-3.32964770695916,0.489931433442046,
-0.932893788903887));
#10950=CARTESIAN_POINT('Ctrl Pts',(-3.26599717460264,1.04969762121448,-0.0919702908041196));
#10951=CARTESIAN_POINT('Ctrl Pts',(-3.20234664224613,0.644694226841407,
0.833482443769645));
#10952=CARTESIAN_POINT('Ctrl Pts',(-3.13869610988962,-0.352843024104558,
0.992887420994864));
#10953=CARTESIAN_POINT('Ctrl Pts',(-3.07504557753311,-1.02608477319307,
0.239736665044628));
#10954=CARTESIAN_POINT('Ctrl Pts',(-3.0113950451766,-0.756259340081533,
-0.733754346404477));
#10955=CARTESIAN_POINT('Ctrl Pts',(-2.94774451282009,0.208638647928818,
-1.03285698184772));
#10956=CARTESIAN_POINT('Ctrl Pts',(-2.88409398046357,0.981778345655356,
-0.382668146504694));
#10957=CARTESIAN_POINT('Ctrl Pts',(-2.82044344810707,0.852572582109705,
0.619228247563606));
#10958=CARTESIAN_POINT('Ctrl Pts',(-2.75679291575055,-0.0602265487918183,
1.05199638458082));
#10959=CARTESIAN_POINT('Ctrl Pts',(-2.69314238339404,-0.917671889104835,
0.51788216255726));
#10960=CARTESIAN_POINT('Ctrl Pts',(-2.62949185103752,-0.931691554229836,
-0.492213854056369));
#10961=CARTESIAN_POINT('Ctrl Pts',(-2.56584131868101,-0.0894001701416109,
-1.04991963498522));
#10962=CARTESIAN_POINT('Ctrl Pts',(-2.5021907863245,0.835058271430786,-0.642651782588028));
#10963=CARTESIAN_POINT('Ctrl Pts',(-2.43854025396799,0.992020623426193,
0.355272730512208));
#10964=CARTESIAN_POINT('Ctrl Pts',(-2.37488972161148,0.237223909848124,
1.02666861593452));
#10965=CARTESIAN_POINT('Ctrl Pts',(-2.31123918925497,-0.735603603964745,
0.754460713478786));
#10966=CARTESIAN_POINT('Ctrl Pts',(-2.24758865689845,-1.03234310232142,
-0.211166639026178));
#10967=CARTESIAN_POINT('Ctrl Pts',(-2.18393812454194,-0.380263432914823,
-0.982712242691651));
#10968=CARTESIAN_POINT('Ctrl Pts',(-2.12028759218543,0.621313640154688,
-0.851054046995969));
#10969=CARTESIAN_POINT('Ctrl Pts',(-2.05663705982892,1.05184578673718,0.0628018412878423));
#10970=CARTESIAN_POINT('Ctrl Pts',(-1.9929865274724,0.515633987688665,0.918937006049595));
#10971=CARTESIAN_POINT('Ctrl Pts',(-1.9293359951159,-0.494493324505228,
0.930483735688552));
#10972=CARTESIAN_POINT('Ctrl Pts',(-1.86568546275938,-1.05013535599715,
0.0868295134890514));
#10973=CARTESIAN_POINT('Ctrl Pts',(-1.80203493040287,-0.640605486555041,
-0.836629094008195));
#10974=CARTESIAN_POINT('Ctrl Pts',(-1.73838439804635,0.357700307590832,
-0.99114788017657));
#10975=CARTESIAN_POINT('Ctrl Pts',(-1.67473386568985,1.02724630519914,-0.234709732754254));
#10976=CARTESIAN_POINT('Ctrl Pts',(-1.61108333333333,0.752657565073169,
0.737448452511809));
#10977=CARTESIAN_POINT('Ctrl Pts',(-1.54743280097682,-0.213693364702976,
1.03182303556954));
#10978=CARTESIAN_POINT('Ctrl Pts',(-1.48378226862031,-0.983640249340781,
0.377856439809512));
#10979=CARTESIAN_POINT('Ctrl Pts',(-1.4201317362638,-0.849530411830376,
-0.623395308143371));
#10980=CARTESIAN_POINT('Ctrl Pts',(-1.35648120390728,0.0653767589075785,
-1.05168888592014));
#10981=CARTESIAN_POINT('Ctrl Pts',(-1.29283067155078,0.92019661236765,-0.513382719774322));
#10982=CARTESIAN_POINT('Ctrl Pts',(-1.22918013919426,0.929270345735347,
0.496769826325492));
#10983=CARTESIAN_POINT('Ctrl Pts',(-1.16552960683775,0.0842583259522808,
1.05034479213317));
#10984=CARTESIAN_POINT('Ctrl Pts',(-1.10187907448124,-0.838194882326415,
0.638555333560757));
#10985=CARTESIAN_POINT('Ctrl Pts',(-1.03822854212472,-0.990269234085938,
-0.360125707666812));
#10986=CARTESIAN_POINT('Ctrl Pts',(-0.974578009768213,-0.232194077407245,
-1.02781790038852));
#10987=CARTESIAN_POINT('Ctrl Pts',(-0.910927477411702,0.739288745424437,
-0.750849786378484));
#10988=CARTESIAN_POINT('Ctrl Pts',(-0.847276945055189,1.03129704196672,
0.216218583445444));
#10989=CARTESIAN_POINT('Ctrl Pts',(-0.783626412698677,0.375446693444177,
0.984562789592695));
#10990=CARTESIAN_POINT('Ctrl Pts',(-0.719975880342165,-0.625472312713079,
0.848000870642187));
#10991=CARTESIAN_POINT('Ctrl Pts',(-0.656325347985652,-1.05152744086089,
-0.0679497395088046));
#10992=CARTESIAN_POINT('Ctrl Pts',(-0.59267481562914,-0.511125036787062,
-0.921453635488242));
#10993=CARTESIAN_POINT('Ctrl Pts',(-0.529024283272629,0.499037016509572,
-0.928045822332354));
#10994=CARTESIAN_POINT('Ctrl Pts',(-0.465373750916116,1.05055995252614,
-0.0816971910864101));
#10995=CARTESIAN_POINT('Ctrl Pts',(-0.401723218559604,0.63647854523422,
0.839775680950435));
#10996=CARTESIAN_POINT('Ctrl Pts',(-0.338072686203093,-0.36250566788185,
0.989346634845035));
#10997=CARTESIAN_POINT('Ctrl Pts',(-0.27442215384658,-1.02846547810574,
0.229749188155657));
#10998=CARTESIAN_POINT('Ctrl Pts',(-0.210771621490069,-0.748881521153355,
-0.741261670011578));
#10999=CARTESIAN_POINT('Ctrl Pts',(-0.147121089133558,0.21844554031981,
-1.03050360978724));
#11000=CARTESIAN_POINT('Ctrl Pts',(-0.0834705567770446,0.986051155088889,
-0.37354034944497));
#11001=CARTESIAN_POINT('Ctrl Pts',(-0.0198200244205324,0.845312008018486,
0.628587983728979));
#11002=CARTESIAN_POINT('Ctrl Pts',(0.0226136638171417,0.236601868752173,
0.908706710441434));
#11003=CARTESIAN_POINT('Ctrl Pts',(0.0438305079359791,-0.0596234658020935,
0.888835794791999));
#11004=CARTESIAN_POINT('Ctrl Pts',(-4.87708050793598,0.474038213689231,
-0.662855146750355));
#11005=CARTESIAN_POINT('Ctrl Pts',(-4.85586366381714,0.694950207510419,
-0.504870815713754));
#11006=CARTESIAN_POINT('Ctrl Pts',(-4.81342997557947,0.962511436578625,
0.0466179265694654));
#11007=CARTESIAN_POINT('Ctrl Pts',(-4.74977944322295,0.480012622195208,
0.836655197545366));
#11008=CARTESIAN_POINT('Ctrl Pts',(-4.68612891086644,-0.444054479343715,
0.855219932190447));
#11009=CARTESIAN_POINT('Ctrl Pts',(-4.62247837850993,-0.959788134663791,
0.0890206716952339));
#11010=CARTESIAN_POINT('Ctrl Pts',(-4.55882784615342,-0.593495978719511,
-0.759655114094331));
#11011=CARTESIAN_POINT('Ctrl Pts',(-4.49517731379691,0.318331319624059,
-0.909791253087425));
#11012=CARTESIAN_POINT('Ctrl Pts',(-4.43152678144039,0.937552417882916,
-0.223927024811924));
#11013=CARTESIAN_POINT('Ctrl Pts',(-4.36787624908388,0.695091682601356,
0.667842975609936));
#11014=CARTESIAN_POINT('Ctrl Pts',(-4.30422571672737,-0.186231226501926,
0.94575265688559));
#11015=CARTESIAN_POINT('Ctrl Pts',(-4.24057518437085,-0.89638593225447,
0.354454502432928));
#11016=CARTESIAN_POINT('Ctrl Pts',(-4.17692465201435,-0.782681059763747,
-0.562634308258189));
#11017=CARTESIAN_POINT('Ctrl Pts',(-4.11327411965783,0.0503816072185008,
-0.96260253959474));
#11018=CARTESIAN_POINT('Ctrl Pts',(-4.04962358730132,0.837138253044138,
-0.477853559646522));
#11019=CARTESIAN_POINT('Ctrl Pts',(-3.98597305494481,0.85448745349913,0.446089269224147));
#11020=CARTESIAN_POINT('Ctrl Pts',(-3.9223225225883,0.0864831625772816,
0.960033554572366));
#11021=CARTESIAN_POINT('Ctrl Pts',(-3.85867199023178,-0.761007090474656,
0.59161843206407));
#11022=CARTESIAN_POINT('Ctrl Pts',(-3.79502145787528,-0.909061214989962,
-0.320549264472495));
#11023=CARTESIAN_POINT('Ctrl Pts',(-3.73137092551876,-0.221603647102998,
-0.938102264149811));
#11024=CARTESIAN_POINT('Ctrl Pts',(-3.66772039316225,0.669528235321151,
-0.693452260557387));
#11025=CARTESIAN_POINT('Ctrl Pts',(-3.60406986080574,0.945301508698372,
0.18854480406292));
#11026=CARTESIAN_POINT('Ctrl Pts',(-3.54041932844923,0.352254917129916,
0.897251663471189));
#11027=CARTESIAN_POINT('Ctrl Pts',(-3.47676879609271,-0.564546649378238,
0.781300943377597));
#11028=CARTESIAN_POINT('Ctrl Pts',(-3.4131182637362,-0.962477426009771,
-0.0527378967020952));
#11029=CARTESIAN_POINT('Ctrl Pts',(-3.34946773137969,-0.47580207812196,
-0.838305709412468));
#11030=CARTESIAN_POINT('Ctrl Pts',(-3.28581719902317,0.44817955917959,-0.853392737295704));
#11031=CARTESIAN_POINT('Ctrl Pts',(-3.22216666666667,0.960242566684416,
-0.0841325981078974));
#11032=CARTESIAN_POINT('Ctrl Pts',(-3.15851613431015,0.589753493384664,
0.762453210254761));
#11033=CARTESIAN_POINT('Ctrl Pts',(-3.09486560195364,-0.32277380100267,
0.908273722161717));
#11034=CARTESIAN_POINT('Ctrl Pts',(-3.03121506959713,-0.93864200159542,
0.219306346816778));
#11035=CARTESIAN_POINT('Ctrl Pts',(-2.96756453724061,-0.691811046459989,
-0.67122392455467));
#11036=CARTESIAN_POINT('Ctrl Pts',(-2.90391400488411,0.190858497483254,
-0.94483708376884));
#11037=CARTESIAN_POINT('Ctrl Pts',(-2.84026347252759,0.898111360352081,
-0.350057231493857));
#11038=CARTESIAN_POINT('Ctrl Pts',(-2.77661294017109,0.779916490219904,
0.566457720572923));
#11039=CARTESIAN_POINT('Ctrl Pts',(-2.71296240781457,-0.0550940524448328,
0.962345429823745));
#11040=CARTESIAN_POINT('Ctrl Pts',(-2.64931187545806,-0.839468045234444,
0.473748331865986));
#11041=CARTESIAN_POINT('Ctrl Pts',(-2.58566134310155,-0.852292956858142,
-0.450267472293478));
#11042=CARTESIAN_POINT('Ctrl Pts',(-2.52201081074503,-0.0817815026954864,
-0.960445660478994));
#11043=CARTESIAN_POINT('Ctrl Pts',(-2.45836027838852,0.76389474614796,-0.587885105886648));
#11044=CARTESIAN_POINT('Ctrl Pts',(-2.39470974603201,0.907480792935895,
0.324996448239377));
#11045=CARTESIAN_POINT('Ctrl Pts',(-2.3310592136755,0.217007728195018,0.939176089356755));
#11046=CARTESIAN_POINT('Ctrl Pts',(-2.26740868131898,-0.672915588697034,
0.690165698513471));
#11047=CARTESIAN_POINT('Ctrl Pts',(-2.20375814896248,-0.944366996969242,
-0.193171053604965));
#11048=CARTESIAN_POINT('Ctrl Pts',(-2.14010761660596,-0.347857447191207,
-0.898965670840194));
#11049=CARTESIAN_POINT('Ctrl Pts',(-2.07645708424945,0.568365396358537,
-0.778527364412868));
#11050=CARTESIAN_POINT('Ctrl Pts',(-2.01280655189294,0.962207665902984,
0.0574498789479774));
#11051=CARTESIAN_POINT('Ctrl Pts',(-1.94915601953643,0.471691746081142,
0.840625349126195));
#11052=CARTESIAN_POINT('Ctrl Pts',(-1.88550548717991,-0.452352686654507,
0.851188068409572));
#11053=CARTESIAN_POINT('Ctrl Pts',(-1.8218549548234,-0.960642997782618,
0.0794299169700061));
#11054=CARTESIAN_POINT('Ctrl Pts',(-1.75820442246689,-0.586013194857034,
-0.76533170348982));
#11055=CARTESIAN_POINT('Ctrl Pts',(-1.69455389011038,0.32721714760812,-0.90668242471905));
#11056=CARTESIAN_POINT('Ctrl Pts',(-1.63090335775387,0.939704548039514,
-0.214707808849747));
#11057=CARTESIAN_POINT('Ctrl Pts',(-1.56725282539735,0.688516214111364,
0.674603219561555));
#11058=CARTESIAN_POINT('Ctrl Pts',(-1.50360229304084,-0.195482452145039,
0.943891250218388));
#11059=CARTESIAN_POINT('Ctrl Pts',(-1.43995176068433,-0.899814592918944,
0.345655577633035));
#11060=CARTESIAN_POINT('Ctrl Pts',(-1.37630122832782,-0.777133573179534,
-0.570269664951738));
#11061=CARTESIAN_POINT('Ctrl Pts',(-1.3126506959713,0.0598053625217287,
-0.962064136147149));
#11062=CARTESIAN_POINT('Ctrl Pts',(-1.2490001636148,0.841777612005919,-0.469632330839386));
#11063=CARTESIAN_POINT('Ctrl Pts',(-1.18534963125828,0.850078083343866,
0.45443518537297));
#11064=CARTESIAN_POINT('Ctrl Pts',(-1.12169909890177,0.0770778456021786,
0.960834585806386));
#11065=CARTESIAN_POINT('Ctrl Pts',(-1.05804856654526,-0.766764055591212,
0.584137755555715));
#11066=CARTESIAN_POINT('Ctrl Pts',(-0.994398034188747,-0.905878656700315,
-0.329435855498018));
#11067=CARTESIAN_POINT('Ctrl Pts',(-0.930747501832234,-0.212406537227819,
-0.940227431983101));
#11068=CARTESIAN_POINT('Ctrl Pts',(-0.867096969475721,0.676286683022042,
-0.686862494012643));
#11069=CARTESIAN_POINT('Ctrl Pts',(-0.80344643711921,0.943410081701831,
0.197792472171475));
#11070=CARTESIAN_POINT('Ctrl Pts',(-0.739795904762698,0.343451189447199,
0.900658514445929));
#11071=CARTESIAN_POINT('Ctrl Pts',(-0.676145372406185,-0.572169667541745,
0.775734379233855));
#11072=CARTESIAN_POINT('Ctrl Pts',(-0.612494840049673,-0.961916449408661,
-0.0621590741493609));
#11073=CARTESIAN_POINT('Ctrl Pts',(-0.548844307693162,-0.467567047216149,
-0.842927511827834));
#11074=CARTESIAN_POINT('Ctrl Pts',(-0.48519377533665,0.456509165991316,
-0.84895791361909));
#11075=CARTESIAN_POINT('Ctrl Pts',(-0.421543242980137,0.961031410266899,
-0.0747349702183289));
#11076=CARTESIAN_POINT('Ctrl Pts',(-0.357892710623625,0.582237950780673,
0.76821013882267));
#11077=CARTESIAN_POINT('Ctrl Pts',(-0.294242178267114,-0.331612995904273,
0.905034681211373));
#11078=CARTESIAN_POINT('Ctrl Pts',(-0.230591645910601,-0.940819823236301,
0.210170001026577));
#11079=CARTESIAN_POINT('Ctrl Pts',(-0.16694111355409,-0.685061964018581,
-0.67809147530807));
#11080=CARTESIAN_POINT('Ctrl Pts',(-0.103290581197579,0.199829648155986,
-0.942684265679081));
#11081=CARTESIAN_POINT('Ctrl Pts',(-0.0396400488410653,0.902020041685152,
-0.34170730376261));
#11082=CARTESIAN_POINT('Ctrl Pts',(0.0240104835154466,0.773274661030189,
0.575019821598291));
#11083=CARTESIAN_POINT('Ctrl Pts',(0.0664441717531208,0.216438697336524,
0.831266877587165));
#11084=CARTESIAN_POINT('Ctrl Pts',(0.0876610158719582,-0.0545423640859427,
0.813089358023476));
#11085=CARTESIAN_POINT('Ctrl Pts',(-4.83325,0.429877377952362,-0.601104350279386));
#11086=CARTESIAN_POINT('Ctrl Pts',(-4.81203315588116,0.630209473381985,
-0.457837651472495));
#11087=CARTESIAN_POINT('Ctrl Pts',(-4.76959946764349,0.872845016829865,
0.0422750560198467));
#11088=CARTESIAN_POINT('Ctrl Pts',(-4.70594893528698,0.435295217673284,
0.758713395217541));
#11089=CARTESIAN_POINT('Ctrl Pts',(-4.64229840293046,-0.402686892608664,
0.775548661280791));
#11090=CARTESIAN_POINT('Ctrl Pts',(-4.57864787057395,-0.870375414479855,
0.0807276118819171));
#11091=CARTESIAN_POINT('Ctrl Pts',(-4.51499733821744,-0.538206599783677,
-0.688886547887163));
#11092=CARTESIAN_POINT('Ctrl Pts',(-4.45134680586093,0.28867595279949,-0.825036182879565));
#11093=CARTESIAN_POINT('Ctrl Pts',(-4.38769627350442,0.850211150606986,
-0.203066249722066));
#11094=CARTESIAN_POINT('Ctrl Pts',(-4.3240457411479,0.63033776882184,0.605627518939458));
#11095=CARTESIAN_POINT('Ctrl Pts',(-4.2603952087914,-0.168882147113114,
0.85764746510496));
#11096=CARTESIAN_POINT('Ctrl Pts',(-4.19674467643488,-0.812879685778983,
0.321433942895504));
#11097=CARTESIAN_POINT('Ctrl Pts',(-4.13309414407837,-0.709767423865924,
-0.510219965807717));
#11098=CARTESIAN_POINT('Ctrl Pts',(-4.06944361172186,0.045688116659549,
-0.872927632797439));
#11099=CARTESIAN_POINT('Ctrl Pts',(-4.00579307936534,0.759151449841031,
-0.433337290821689));
#11100=CARTESIAN_POINT('Ctrl Pts',(-3.94214254700883,0.774884419432483,
0.404532123885857));
#11101=CARTESIAN_POINT('Ctrl Pts',(-3.87849201465232,0.0784264940929817,
0.870597971361873));
#11102=CARTESIAN_POINT('Ctrl Pts',(-3.8148414822958,-0.690112575757162,
0.536503963139801));
#11103=CARTESIAN_POINT('Ctrl Pts',(-3.7511909499393,-0.824374154262293,
-0.290687276545878));
#11104=CARTESIAN_POINT('Ctrl Pts',(-3.68754041758278,-0.200959315114973,
-0.850709773850142));
#11105=CARTESIAN_POINT('Ctrl Pts',(-3.62388988522628,0.607155781861951,
-0.628851073384074));
#11106=CARTESIAN_POINT('Ctrl Pts',(-3.56023935286976,0.857238345345858,
0.170980194542391));
#11107=CARTESIAN_POINT('Ctrl Pts',(-3.49658882051325,0.319439268341143,
0.813664766506036));
#11108=CARTESIAN_POINT('Ctrl Pts',(-3.43293828815674,-0.511954155505293,
0.708515877479547));
#11109=CARTESIAN_POINT('Ctrl Pts',(-3.36928775580022,-0.872814174645122,
-0.0478248970195566));
#11110=CARTESIAN_POINT('Ctrl Pts',(-3.30563722344371,-0.431476922874065,
-0.760210147363717));
#11111=CARTESIAN_POINT('Ctrl Pts',(-3.2419866910872,0.406427684917135,-0.773891685687522));
#11112=CARTESIAN_POINT('Ctrl Pts',(-3.17833615873069,0.870787512154351,
-0.0762949054116745));
#11113=CARTESIAN_POINT('Ctrl Pts',(-3.11468562637417,0.534812759927923,
0.691423976739877));
#11114=CARTESIAN_POINT('Ctrl Pts',(-3.05103509401767,-0.292704577900781,
0.82366002332857));
#11115=CARTESIAN_POINT('Ctrl Pts',(-2.98738456166115,-0.85119922999777,
0.198876028588928));
#11116=CARTESIAN_POINT('Ctrl Pts',(-2.92373402930464,-0.627362752838443,
-0.608693502704864));
#11117=CARTESIAN_POINT('Ctrl Pts',(-2.86008349694812,0.173078347037689,
-0.856817185689954));
#11118=CARTESIAN_POINT('Ctrl Pts',(-2.79643296459162,0.814444375048807,
-0.317446316483022));
#11119=CARTESIAN_POINT('Ctrl Pts',(-2.7327824322351,0.707260398330102,0.513687193582241));
#11120=CARTESIAN_POINT('Ctrl Pts',(-2.66913189987859,-0.0499615560978463,
0.872694475066671));
#11121=CARTESIAN_POINT('Ctrl Pts',(-2.60548136752208,-0.761264201364054,
0.429614501174711));
#11122=CARTESIAN_POINT('Ctrl Pts',(-2.54183083516557,-0.772894359486448,
-0.408321090530588));
#11123=CARTESIAN_POINT('Ctrl Pts',(-2.47818030280905,-0.0741628352493615,
-0.870971685972771));
#11124=CARTESIAN_POINT('Ctrl Pts',(-2.41452977045254,0.692731220865135,
-0.533118429185269));
#11125=CARTESIAN_POINT('Ctrl Pts',(-2.35087923809603,0.822940962445597,
0.294720165966547));
#11126=CARTESIAN_POINT('Ctrl Pts',(-2.28722870573952,0.196791546541912,
0.851683562778987));
#11127=CARTESIAN_POINT('Ctrl Pts',(-2.22357817338301,-0.610227573429323,
0.625870683548156));
#11128=CARTESIAN_POINT('Ctrl Pts',(-2.1599276410265,-0.856390891617059,
-0.175175468183749));
#11129=CARTESIAN_POINT('Ctrl Pts',(-2.09627710866998,-0.31545146146759,
-0.815219098988737));
#11130=CARTESIAN_POINT('Ctrl Pts',(-2.03262657631347,0.515417152562384,
-0.706000681829764));
#11131=CARTESIAN_POINT('Ctrl Pts',(-1.96897604395696,0.872569545068786,
0.0520979166081116));
#11132=CARTESIAN_POINT('Ctrl Pts',(-1.90532551160045,0.427749504473617,
0.762313692202795));
#11133=CARTESIAN_POINT('Ctrl Pts',(-1.84167497924393,-0.410212048803786,
0.771892401130592));
#11134=CARTESIAN_POINT('Ctrl Pts',(-1.77802444688742,-0.871150639568081,
0.0720303204509612));
#11135=CARTESIAN_POINT('Ctrl Pts',(-1.71437391453091,-0.531420903159026,
-0.694034312971445));
#11136=CARTESIAN_POINT('Ctrl Pts',(-1.6507233821744,0.296733987625408,-0.822216969261532));
#11137=CARTESIAN_POINT('Ctrl Pts',(-1.58707284981789,0.852162790879889,
-0.194705884945239));
#11138=CARTESIAN_POINT('Ctrl Pts',(-1.52342231746138,0.624374863149558,
0.611757986611301));
#11139=CARTESIAN_POINT('Ctrl Pts',(-1.45977178510486,-0.177271539587102,
0.85595946486723));
#11140=CARTESIAN_POINT('Ctrl Pts',(-1.39612125274835,-0.815988936497109,
0.313454715456559));
#11141=CARTESIAN_POINT('Ctrl Pts',(-1.33247072039184,-0.70473673452869,
-0.517144021760104));
#11142=CARTESIAN_POINT('Ctrl Pts',(-1.26882018803533,0.0542339661358782,
-0.872439386374161));
#11143=CARTESIAN_POINT('Ctrl Pts',(-1.20516965567882,0.763358611644189,
-0.42588194190445));
#11144=CARTESIAN_POINT('Ctrl Pts',(-1.1415191233223,0.770885820952385,0.412100544420447));
#11145=CARTESIAN_POINT('Ctrl Pts',(-1.07786859096579,0.0698973652520763,
0.871324379479602));
#11146=CARTESIAN_POINT('Ctrl Pts',(-1.01421805860928,-0.695333228856009,
0.529720177550673));
#11147=CARTESIAN_POINT('Ctrl Pts',(-0.950567526252767,-0.821488079314692,
-0.298746003329225));
#11148=CARTESIAN_POINT('Ctrl Pts',(-0.886916993896255,-0.192618997048393,
-0.852636963577682));
#11149=CARTESIAN_POINT('Ctrl Pts',(-0.823266461539743,0.613284620619645,
-0.622875201646802));
#11150=CARTESIAN_POINT('Ctrl Pts',(-0.759615929183231,0.855523121436939,
0.179366360897505));
#11151=CARTESIAN_POINT('Ctrl Pts',(-0.695965396826718,0.311455685450219,
0.816754239299164));
#11152=CARTESIAN_POINT('Ctrl Pts',(-0.632314864470207,-0.51886702237041,
0.703467887825523));
#11153=CARTESIAN_POINT('Ctrl Pts',(-0.568664332113694,-0.872305457956439,
-0.0563684087899174));
#11154=CARTESIAN_POINT('Ctrl Pts',(-0.505013799757182,-0.424009057645233,
-0.764401388167426));
#11155=CARTESIAN_POINT('Ctrl Pts',(-0.441363267400671,0.413981315473058,
-0.769870004905825));
#11156=CARTESIAN_POINT('Ctrl Pts',(-0.377712735044158,0.871502868007656,
-0.0677727493502481));
#11157=CARTESIAN_POINT('Ctrl Pts',(-0.314062202687646,0.527997356327125,
0.696644596694906));
#11158=CARTESIAN_POINT('Ctrl Pts',(-0.250411670331135,-0.300720323926695,
0.82072272757771));
#11159=CARTESIAN_POINT('Ctrl Pts',(-0.186761137974622,-0.853174168366862,
0.190590813897497));
#11160=CARTESIAN_POINT('Ctrl Pts',(-0.123110605618111,-0.621242406883804,
-0.614921280604562));
#11161=CARTESIAN_POINT('Ctrl Pts',(-0.0594600732615994,0.181213755992161,
-0.854864921570925));
#11162=CARTESIAN_POINT('Ctrl Pts',(0.00419045909491373,0.817988928281414,
-0.309874258080251));
#11163=CARTESIAN_POINT('Ctrl Pts',(0.0678409914514257,0.701237314041894,
0.521451659467605));
#11164=CARTESIAN_POINT('Ctrl Pts',(0.1102746796891,0.196275525920875,0.753827044732897));
#11165=CARTESIAN_POINT('Ctrl Pts',(0.131491523807937,-0.0494612623697919,
0.737342921254952));
#11166=CARTESIAN_POINT('',(0.,-0.0647045675182444,0.964582231560522));
#11167=CARTESIAN_POINT('Ctrl Pts',(1.33226762955019E-15,0.673678098462144,
-0.306812656843374));
#11168=CARTESIAN_POINT('Ctrl Pts',(1.26162819850666E-15,0.682701071734832,
-0.293075508768413));
#11169=CARTESIAN_POINT('Ctrl Pts',(2.45173685381688E-15,0.691216371063901,
-0.279039978129302));
#11170=CARTESIAN_POINT('Ctrl Pts',(1.9151347174784E-15,0.699201547817293,
-0.264726438657214));
#11171=CARTESIAN_POINT('Ctrl Pts',(8.16496915529504E-16,0.715544774938514,
-0.235430978616017));
#11172=CARTESIAN_POINT('Ctrl Pts',(-7.04589669016225E-16,0.729669893758505,
-0.204973366286778));
#11173=CARTESIAN_POINT('Ctrl Pts',(-1.4432899320127E-15,0.741647292599094,
-0.173608377626765));
#11174=CARTESIAN_POINT('Ctrl Pts',(-1.81000055251089E-15,0.747593194585063,
-0.158037956131618));
#11175=CARTESIAN_POINT('Ctrl Pts',(-6.71930333473227E-17,0.75300928099856,
-0.142243325776783));
#11176=CARTESIAN_POINT('Ctrl Pts',(8.32667268468867E-17,0.757900867432782,
-0.126252678619381));
#11177=CARTESIAN_POINT('Ctrl Pts',(1.65288103861796E-16,0.760567458517365,
-0.117535564505171));
#11178=CARTESIAN_POINT('Ctrl Pts',(4.25358405107105E-16,0.7630755185763,
-0.108768611274642));
#11179=CARTESIAN_POINT('Ctrl Pts',(3.19189119579733E-16,0.765425760805947,
-0.0999598388073907));
#11180=CARTESIAN_POINT('Ctrl Pts',(-9.74340084487751E-17,0.774648440081561,
-0.0653929834200916));
#11181=CARTESIAN_POINT('Ctrl Pts',(-1.59689830842923E-15,0.781448636241036,
-0.0301702542091566));
#11182=CARTESIAN_POINT('Ctrl Pts',(-1.72084568816899E-15,0.785898139234381,
0.0054248396438656));
#11183=CARTESIAN_POINT('Ctrl Pts',(-1.77326446796872E-15,0.787779885489252,
0.0204784163354387));
#11184=CARTESIAN_POINT('Ctrl Pts',(-1.13606037005565E-16,0.789240689578657,
0.0355990132743527));
#11185=CARTESIAN_POINT('Ctrl Pts',(2.77555756156289E-17,0.790283669830199,
0.0507667158925832));
#11186=CARTESIAN_POINT('Ctrl Pts',(1.22708800898342E-16,0.790984244313992,
0.0609549293475994));
#11187=CARTESIAN_POINT('Ctrl Pts',(-1.83521606155334E-15,0.791496273356183,
0.0711644128913534));
#11188=CARTESIAN_POINT('Ctrl Pts',(-1.94289029309402E-15,0.791820338514077,
0.0813892836455744));
#11189=CARTESIAN_POINT('Ctrl Pts',(-2.0287791605619E-15,0.792078836661675,
0.0895453907894976));
#11190=CARTESIAN_POINT('Ctrl Pts',(-8.04773162025033E-16,0.792217424127839,
0.0977019226404007));
#11191=CARTESIAN_POINT('Ctrl Pts',(-7.63278329429795E-16,0.792237110441147,
0.105854814370456));
#11192=CARTESIAN_POINT('Ctrl Pts',(-5.70752003916141E-16,0.792328450334021,
0.143682326591298));
#11193=CARTESIAN_POINT('Ctrl Pts',(6.91671501508328E-16,0.789864079330926,
0.181435048362651));
#11194=CARTESIAN_POINT('Ctrl Pts',(4.16333634234434E-16,0.784919243793111,
0.218809898022086));
#11195=CARTESIAN_POINT('Ctrl Pts',(1.39195737996481E-16,0.779942081255458,
0.256429086800511));
#11196=CARTESIAN_POINT('Ctrl Pts',(-1.2864070917373E-15,0.772452165960967,
0.293666812246517));
#11197=CARTESIAN_POINT('Ctrl Pts',(-1.08246744900953E-15,0.762476389798144,
0.330232150500554));
#11198=CARTESIAN_POINT('Ctrl Pts',(-9.77539916565035E-16,0.757343824285215,
0.349045122145874));
#11199=CARTESIAN_POINT('Ctrl Pts',(-8.98682738517916E-16,0.751552389328626,
0.367680271279987));
#11200=CARTESIAN_POINT('Ctrl Pts',(-7.63278329429795E-16,0.745100333168384,
0.386097971021693));
#11201=CARTESIAN_POINT('Ctrl Pts',(-7.09222220555815E-16,0.742524545181805,
0.393450679763976));
#11202=CARTESIAN_POINT('Ctrl Pts',(-1.06852512968364E-15,0.739843366987135,
0.400768487743));
#11203=CARTESIAN_POINT('Ctrl Pts',(-1.01307850997046E-15,0.737061996657759,
0.408035709516201));
#11204=CARTESIAN_POINT('Ctrl Pts',(-7.41575990705545E-16,0.723442608220004,
0.443620728579352));
#11205=CARTESIAN_POINT('Ctrl Pts',(1.3251228527546E-16,0.707397104602246,
0.478072699106861));
#11206=CARTESIAN_POINT('Ctrl Pts',(-1.38777878078145E-17,0.688976337650526,
0.511110601292894));
#11207=CARTESIAN_POINT('Ctrl Pts',(-1.61067221558875E-16,0.670508669475494,
0.544232621476414));
#11208=CARTESIAN_POINT('Ctrl Pts',(5.04848495992574E-16,0.649654206725436,
0.575935028571295));
#11209=CARTESIAN_POINT('Ctrl Pts',(4.02455846426619E-16,0.626669853806303,
0.606134845516811));
#11210=CARTESIAN_POINT('Ctrl Pts',(3.53818460908109E-16,0.615752089312853,
0.620480017221947));
#11211=CARTESIAN_POINT('Ctrl Pts',(1.90633954196E-16,0.604352983851072,
0.634485939752549));
#11212=CARTESIAN_POINT('Ctrl Pts',(4.85722573273506E-17,0.592496253768456,
0.648142208249025));
#11213=CARTESIAN_POINT('Ctrl Pts',(-3.70262688802134E-17,0.585352043590175,
0.65637072080772));
#11214=CARTESIAN_POINT('Ctrl Pts',(5.68400082910913E-16,0.578041643527712,
0.664472266409089));
#11215=CARTESIAN_POINT('Ctrl Pts',(5.62050406216485E-16,0.570569866093675,
0.672444343598201));
#11216=CARTESIAN_POINT('Ctrl Pts',(5.57365453966068E-16,0.565056999503958,
0.678326344015705));
#11217=CARTESIAN_POINT('Ctrl Pts',(2.54124751848738E-16,0.559462767422932,
0.68413090343335));
#11218=CARTESIAN_POINT('Ctrl Pts',(2.4980018054066E-16,0.55379130780884,
0.689855844240334));
#11219=CARTESIAN_POINT('Ctrl Pts',(2.2854393084537E-16,0.525914796333886,
0.717995227919058));
#11220=CARTESIAN_POINT('Ctrl Pts',(-5.13507583854888E-16,0.496165136066849,
0.744224704620086));
#11221=CARTESIAN_POINT('Ctrl Pts',(-7.0082828429463E-16,0.464828529226713,
0.768461197317664));
#11222=CARTESIAN_POINT('Ctrl Pts',(-8.92479401630727E-16,0.432767493258262,
0.793257981094869));
#11223=CARTESIAN_POINT('Ctrl Pts',(1.05793968957062E-15,0.399044594950855,
0.815969430632288));
#11224=CARTESIAN_POINT('Ctrl Pts',(1.64104840827406E-15,0.363917889441643,
0.836481655737946));
#11225=CARTESIAN_POINT('Ctrl Pts',(1.92123829438634E-15,0.347039137160234,
0.846337996128539));
#11226=CARTESIAN_POINT('Ctrl Pts',(3.50655276928491E-16,0.329835617352691,
0.855686110955217));
#11227=CARTESIAN_POINT('Ctrl Pts',(3.98986399474666E-16,0.312332888405914,
0.864510465234708));
#11228=CARTESIAN_POINT('Ctrl Pts',(4.20291846343656E-16,0.304617291457351,
0.868400439258697));
#11229=CARTESIAN_POINT('Ctrl Pts',(1.74879569696092E-16,0.296843528570104,
0.872188605992907));
#11230=CARTESIAN_POINT('Ctrl Pts',(2.1163626406917E-16,0.289013692376419,
0.875873495777978));
#11231=CARTESIAN_POINT('Ctrl Pts',(2.46655081879023E-16,0.281554055109676,
0.879384161963654));
#11232=CARTESIAN_POINT('Ctrl Pts',(6.15661485392124E-16,0.274052281453019,
0.882796944360599));
#11233=CARTESIAN_POINT('Ctrl Pts',(6.03683769639929E-16,0.266512258373315,
0.886110438059811));
#11234=CARTESIAN_POINT('Ctrl Pts',(5.42137320242176E-16,0.227768506347988,
0.903136536900986));
#11235=CARTESIAN_POINT('Ctrl Pts',(-1.52944883977296E-16,0.188004613069195,
0.917550080046915));
#11236=CARTESIAN_POINT('Ctrl Pts',(-2.16840434497101E-16,0.147507771680282,
0.929243019478543));
#11237=CARTESIAN_POINT('Ctrl Pts',(-2.80291741920052E-16,0.107292490463947,
0.940854662050183));
#11238=CARTESIAN_POINT('Ctrl Pts',(-2.94422254401383E-16,0.0663533628840327,
0.949784153433247));
#11239=CARTESIAN_POINT('Ctrl Pts',(-1.53523027623947E-16,0.0249389809248478,
0.955887516550197));
#11240=CARTESIAN_POINT('Ctrl Pts',(-5.25968927274823E-17,-0.00472614638538816,
0.960259356363317));
#11241=CARTESIAN_POINT('Ctrl Pts',(-6.68384999314338E-17,-0.0346358430448255,
0.963180394324237));
#11242=CARTESIAN_POINT('Ctrl Pts',(0.,-0.0647045675182443,0.964582231560522));
#11243=CARTESIAN_POINT('Ctrl Pts',(0.,-0.0647045675182444,0.964582231560522));
#11244=CARTESIAN_POINT('Ctrl Pts',(-0.0212168441188374,0.256765040167821,
0.986146543295702));
#11245=CARTESIAN_POINT('Ctrl Pts',(-0.0424336882376745,0.587057197587301,
0.834151344577684));
#11246=CARTESIAN_POINT('Ctrl Pts',(-0.0636505323565117,0.777658761878016,
0.576898821720842));
#11247=CARTESIAN_POINT('Ctrl Pts',(-0.0848673764753489,0.96826032616873,
0.319646298864001));
#11248=CARTESIAN_POINT('Ctrl Pts',(-0.106084220594186,1.01917129733068,
-0.0428635481316647));
#11249=CARTESIAN_POINT('Ctrl Pts',(-0.127301064713024,0.905789976910154,
-0.342943398090841));
#11250=CARTESIAN_POINT('Ctrl Pts',(-0.148517908831861,0.792408656489629,
-0.643023248050018));
#11251=CARTESIAN_POINT('Ctrl Pts',(-0.169734752950699,0.514735044486632,
-0.880673100972706));
#11252=CARTESIAN_POINT('Ctrl Pts',(-0.190951597069536,0.200937820023172,
-0.947182845903998));
#11253=CARTESIAN_POINT('Ctrl Pts',(-0.212168441188374,-0.112859404440287,
-1.01369259083529));
#11254=CARTESIAN_POINT('Ctrl Pts',(-0.233385285307211,-0.462780241364209,
-0.909062227775188));
#11255=CARTESIAN_POINT('Ctrl Pts',(-0.254602129426048,-0.688309002274012,
-0.681120339578499));
#11256=CARTESIAN_POINT('Ctrl Pts',(-0.271156113987472,-0.864272948907491,
-0.503273602477781));
#11257=CARTESIAN_POINT('Ctrl Pts',(-0.287710098548895,-0.964512426583853,
-0.25036018865241));
#11258=CARTESIAN_POINT('Ctrl Pts',(-0.304264083110319,-0.966880390654327,
0.000888722329053411));
#11259=CARTESIAN_POINT('Origin',(1.6,-0.25,-1.1));
#11260=CARTESIAN_POINT('',(1.6,-0.25,-0.25));
#11261=CARTESIAN_POINT('',(0.7,-0.25,-0.25));
#11262=CARTESIAN_POINT('',(1.6,-0.25,-0.25));
#11263=CARTESIAN_POINT('',(1.6,-0.25,-1.1));
#11264=CARTESIAN_POINT('',(1.6,-0.25,-0.55));
#11265=CARTESIAN_POINT('',(0.7,-0.25,-1.1));
#11266=CARTESIAN_POINT('',(1.6,-0.25,-1.1));
#11267=CARTESIAN_POINT('',(0.7,-0.25,-1.1));
#11268=CARTESIAN_POINT('Origin',(1.6,0.25,1.1));
#11269=CARTESIAN_POINT('',(0.7,0.25,-0.25));
#11270=CARTESIAN_POINT('',(1.6,0.25,-0.25));
#11271=CARTESIAN_POINT('',(1.6,0.25,-0.25));
#11272=CARTESIAN_POINT('',(0.7,0.25,-1.1));
#11273=CARTESIAN_POINT('',(0.7,0.25,1.1));
#11274=CARTESIAN_POINT('',(1.6,0.25,-1.1));
#11275=CARTESIAN_POINT('',(1.6,0.25,-1.1));
#11276=CARTESIAN_POINT('',(1.6,0.25,0.55));
#11277=CARTESIAN_POINT('Origin',(1.6,0.25,1.1));
#11278=CARTESIAN_POINT('',(1.6,0.25,0.25));
#11279=CARTESIAN_POINT('',(0.7,0.25,0.25));
#11280=CARTESIAN_POINT('',(1.6,0.25,0.25));
#11281=CARTESIAN_POINT('',(1.6,0.25,1.1));
#11282=CARTESIAN_POINT('',(1.6,0.25,0.55));
#11283=CARTESIAN_POINT('',(0.7,0.25,1.1));
#11284=CARTESIAN_POINT('',(1.6,0.25,1.1));
#11285=CARTESIAN_POINT('',(0.7,0.25,1.1));
#11286=CARTESIAN_POINT('Origin',(1.6,-0.25,1.1));
#11287=CARTESIAN_POINT('',(1.6,-0.25,1.1));
#11288=CARTESIAN_POINT('',(1.6,-0.125,1.1));
#11289=CARTESIAN_POINT('',(0.7,-0.25,1.1));
#11290=CARTESIAN_POINT('',(1.6,-0.25,1.1));
#11291=CARTESIAN_POINT('',(0.7,-0.25,1.1));
#11292=CARTESIAN_POINT('Origin',(1.6,-0.25,-1.1));
#11293=CARTESIAN_POINT('',(0.7,-0.25,0.25));
#11294=CARTESIAN_POINT('',(1.6,-0.25,0.25));
#11295=CARTESIAN_POINT('',(1.6,-0.25,0.25));
#11296=CARTESIAN_POINT('',(0.7,-0.25,-1.1));
#11297=CARTESIAN_POINT('',(1.6,-0.25,-0.55));
#11298=CARTESIAN_POINT('Origin',(1.6,0.25,-1.1));
#11299=CARTESIAN_POINT('',(1.6,0.125,-1.1));
#11300=CARTESIAN_POINT('',(0.7,0.25,-1.1));
#11301=CARTESIAN_POINT('Origin',(1.6,-1.1,0.25));
#11302=CARTESIAN_POINT('',(0.7,1.1,0.25));
#11303=CARTESIAN_POINT('',(0.7,-1.1,0.25));
#11304=CARTESIAN_POINT('',(1.6,1.1,0.25));
#11305=CARTESIAN_POINT('',(1.6,1.1,0.25));
#11306=CARTESIAN_POINT('',(1.6,-0.55,0.25));
#11307=CARTESIAN_POINT('Origin',(1.6,0.,0.));
#11308=CARTESIAN_POINT('',(1.6,-1.6,-1.95943487863577E-16));
#11309=CARTESIAN_POINT('Origin',(1.6,0.,0.));
#11310=CARTESIAN_POINT('',(1.6,1.1,-0.25));
#11311=CARTESIAN_POINT('',(1.6,1.1,0.125));
#11312=CARTESIAN_POINT('',(1.6,0.55,-0.25));
#11313=CARTESIAN_POINT('',(1.6,-1.1,-0.25));
#11314=CARTESIAN_POINT('',(1.6,0.55,-0.25));
#11315=CARTESIAN_POINT('',(1.6,-1.1,0.25));
#11316=CARTESIAN_POINT('',(1.6,-1.1,-0.125));
#11317=CARTESIAN_POINT('',(1.6,-0.55,0.25));
#11318=CARTESIAN_POINT('Origin',(1.6,1.1,-0.25));
#11319=CARTESIAN_POINT('',(0.7,1.1,-0.25));
#11320=CARTESIAN_POINT('',(1.6,1.1,-0.25));
#11321=CARTESIAN_POINT('',(0.7,1.1,-0.25));
#11322=CARTESIAN_POINT('Origin',(1.6,1.1,0.25));
#11323=CARTESIAN_POINT('',(0.7,1.1,0.25));
#11324=CARTESIAN_POINT('Origin',(1.6,-1.1,0.25));
#11325=CARTESIAN_POINT('',(0.7,-1.1,0.25));
#11326=CARTESIAN_POINT('',(1.6,-1.1,0.25));
#11327=CARTESIAN_POINT('',(0.7,-1.1,0.25));
#11328=CARTESIAN_POINT('Origin',(1.6,-1.1,-0.25));
#11329=CARTESIAN_POINT('',(0.7,-1.1,-0.25));
#11330=CARTESIAN_POINT('',(1.6,-1.1,-0.25));
#11331=CARTESIAN_POINT('',(0.7,-1.1,-0.25));
#11332=CARTESIAN_POINT('Origin',(1.6,1.1,-0.25));
#11333=CARTESIAN_POINT('',(0.7,1.1,-0.25));
#11334=CARTESIAN_POINT('Origin',(0.7,0.,0.));
#11335=CARTESIAN_POINT('Origin',(-5.,0.8,0.));
#11336=CARTESIAN_POINT('',(-5.,-0.8,-9.79717439317883E-17));
#11337=CARTESIAN_POINT('Origin',(-5.,0.,0.));
#11338=CARTESIAN_POINT('Origin',(-4.9,0.,0.));
#11339=CARTESIAN_POINT('',(-4.9,-0.9,-1.10218211923262E-16));
#11340=CARTESIAN_POINT('Origin',(-2.4,0.,0.));
#11341=CARTESIAN_POINT('Origin',(0.,0.,0.));
#11342=CARTESIAN_POINT('Origin',(0.,2.,0.));
#11343=CARTESIAN_POINT('',(0.,-2.,-2.44929359829471E-16));
#11344=CARTESIAN_POINT('Origin',(0.,0.,0.));
#11345=CARTESIAN_POINT('Origin',(0.55,0.,0.));
#11346=CARTESIAN_POINT('',(1.1,-2.,-2.44929359829471E-16));
#11347=CARTESIAN_POINT('Origin',(1.1,0.,0.));
#11348=CARTESIAN_POINT('',(0.55,-2.,-2.44929359829471E-16));
#11349=CARTESIAN_POINT('Origin',(1.35,0.,0.));
#11350=CARTESIAN_POINT('',(1.35,-1.8,-2.20436423846524E-16));
#11351=CARTESIAN_POINT('',(0.,0.,0.));
#11352=CARTESIAN_POINT('Origin',(0.1,0.,0.));
#11353=CARTESIAN_POINT('',(0.,1.45,-1.77573785876366E-16));
#11354=CARTESIAN_POINT('Origin',(0.,0.,0.));
#11355=CARTESIAN_POINT('',(0.2,1.25,1.53080849893419E-16));
#11356=CARTESIAN_POINT('',(0.1,1.35,-1.65327317884893E-16));
#11357=CARTESIAN_POINT('',(0.2,-1.25,-1.53080849893419E-16));
#11358=CARTESIAN_POINT('Origin',(0.2,0.,0.));
#11359=CARTESIAN_POINT('Origin',(0.2,0.,0.));
#11360=CARTESIAN_POINT('Origin',(3.4,0.,0.));
#11361=CARTESIAN_POINT('',(6.6,1.25,-1.53080849893419E-16));
#11362=CARTESIAN_POINT('',(6.6,-1.25,-1.53080849893419E-16));
#11363=CARTESIAN_POINT('Origin',(6.6,0.,0.));
#11364=CARTESIAN_POINT('Origin',(6.6,0.,0.));
#11365=CARTESIAN_POINT('',(3.4,-1.25,-1.53080849893419E-16));
#11366=CARTESIAN_POINT('Origin',(0.,1.8,0.));
#11367=CARTESIAN_POINT('',(1.73472347597681E-17,-1.8,-2.20436423846524E-16));
#11368=CARTESIAN_POINT('Origin',(0.,0.,0.));
#11369=CARTESIAN_POINT('Origin',(6.7,0.,0.));
#11370=CARTESIAN_POINT('',(6.8,1.45,1.77573785876366E-16));
#11371=CARTESIAN_POINT('',(6.7,1.35,-1.65327317884893E-16));
#11372=CARTESIAN_POINT('Origin',(6.8,0.,0.));
#11373=CARTESIAN_POINT('Origin',(6.8,1.25,0.));
#11374=CARTESIAN_POINT('',(6.8,-1.8,-2.20436423846524E-16));
#11375=CARTESIAN_POINT('Origin',(6.8,0.,0.));
#11376=CARTESIAN_POINT('Origin',(0.1,0.,0.));
#11377=CARTESIAN_POINT('',(0.2,-2.,-2.44929359829471E-16));
#11378=CARTESIAN_POINT('Origin',(0.2,0.,0.));
#11379=CARTESIAN_POINT('',(0.1,-1.9,-2.32682891837997E-16));
#11380=CARTESIAN_POINT('Origin',(3.4,0.,0.));
#11381=CARTESIAN_POINT('',(6.6,-2.,-2.44929359829471E-16));
#11382=CARTESIAN_POINT('Origin',(6.6,0.,0.));
#11383=CARTESIAN_POINT('',(3.4,-2.,-2.44929359829471E-16));
#11384=CARTESIAN_POINT('Origin',(6.7,0.,0.));
#11385=CARTESIAN_POINT('',(6.7,-1.9,-2.32682891837997E-16));
#11386=CARTESIAN_POINT('',(0.,0.,0.));
#11387=CARTESIAN_POINT('',(0.,0.,0.));
#11388=CARTESIAN_POINT('',(0.,0.,0.));
#11389=CARTESIAN_POINT('',(0.,0.,6.));
#11390=CARTESIAN_POINT('',(0.,0.,9.));
#11391=CARTESIAN_POINT('',(0.,0.,0.));
#11392=CARTESIAN_POINT('',(-8.32667268468867E-16,5.6,10.75));
#11393=CARTESIAN_POINT('',(0.,-8.2,4.));
#11394=CARTESIAN_POINT('',(0.,0.,0.));
#11395=CARTESIAN_POINT('',(-1.09287578986539E-16,2.22044604925031E-16,0.));
#11396=CARTESIAN_POINT('',(-12.,0.,9.4));
#11397=CARTESIAN_POINT('',(-12.,0.,12.5));
#11398=CARTESIAN_POINT('',(-18.,-3.40000000000003,-6.));
#11399=CARTESIAN_POINT('',(8.50014503228635E-17,-1.11022302462516E-16,0.));
#11400=CARTESIAN_POINT('',(12.,0.,9.4));
#11401=CARTESIAN_POINT('',(12.,0.,12.5));
#11402=CARTESIAN_POINT('',(18.,-3.40000000000001,-6.));
#11403=UNCERTAINTY_MEASURE_WITH_UNIT(LENGTH_MEASURE(0.01),#11431,
'DISTANCE_ACCURACY_VALUE',
'Maximum model space distance between geometric entities at asserted c
onnectivities');
#11404=UNCERTAINTY_MEASURE_WITH_UNIT(LENGTH_MEASURE(0.01),#11431,
'DISTANCE_ACCURACY_VALUE',
'Maximum model space distance between geometric entities at asserted c
onnectivities');
#11405=UNCERTAINTY_MEASURE_WITH_UNIT(LENGTH_MEASURE(0.01),#11431,
'DISTANCE_ACCURACY_VALUE',
'Maximum model space distance between geometric entities at asserted c
onnectivities');
#11406=UNCERTAINTY_MEASURE_WITH_UNIT(LENGTH_MEASURE(0.01),#11431,
'DISTANCE_ACCURACY_VALUE',
'Maximum model space distance between geometric entities at asserted c
onnectivities');
#11407=UNCERTAINTY_MEASURE_WITH_UNIT(LENGTH_MEASURE(0.01),#11431,
'DISTANCE_ACCURACY_VALUE',
'Maximum model space distance between geometric entities at asserted c
onnectivities');
#11408=UNCERTAINTY_MEASURE_WITH_UNIT(LENGTH_MEASURE(0.01),#11431,
'DISTANCE_ACCURACY_VALUE',
'Maximum model space distance between geometric entities at asserted c
onnectivities');
#11409=UNCERTAINTY_MEASURE_WITH_UNIT(LENGTH_MEASURE(0.01),#11431,
'DISTANCE_ACCURACY_VALUE',
'Maximum model space distance between geometric entities at asserted c
onnectivities');
#11410=UNCERTAINTY_MEASURE_WITH_UNIT(LENGTH_MEASURE(0.01),#11431,
'DISTANCE_ACCURACY_VALUE',
'Maximum model space distance between geometric entities at asserted c
onnectivities');
#11411=UNCERTAINTY_MEASURE_WITH_UNIT(LENGTH_MEASURE(0.01),#11431,
'DISTANCE_ACCURACY_VALUE',
'Maximum model space distance between geometric entities at asserted c
onnectivities');
#11412=UNCERTAINTY_MEASURE_WITH_UNIT(LENGTH_MEASURE(0.01),#11431,
'DISTANCE_ACCURACY_VALUE',
'Maximum model space distance between geometric entities at asserted c
onnectivities');
#11413=UNCERTAINTY_MEASURE_WITH_UNIT(LENGTH_MEASURE(0.01),#11431,
'DISTANCE_ACCURACY_VALUE',
'Maximum model space distance between geometric entities at asserted c
onnectivities');
#11414=UNCERTAINTY_MEASURE_WITH_UNIT(LENGTH_MEASURE(0.01),#11431,
'DISTANCE_ACCURACY_VALUE',
'Maximum model space distance between geometric entities at asserted c
onnectivities');
#11415=UNCERTAINTY_MEASURE_WITH_UNIT(LENGTH_MEASURE(0.01),#11431,
'DISTANCE_ACCURACY_VALUE',
'Maximum model space distance between geometric entities at asserted c
onnectivities');
#11416=UNCERTAINTY_MEASURE_WITH_UNIT(LENGTH_MEASURE(0.01),#11431,
'DISTANCE_ACCURACY_VALUE',
'Maximum model space distance between geometric entities at asserted c
onnectivities');
#11417=(
GEOMETRIC_REPRESENTATION_CONTEXT(3)
GLOBAL_UNCERTAINTY_ASSIGNED_CONTEXT((#11403))
GLOBAL_UNIT_ASSIGNED_CONTEXT((#11431,#11433,#11434))
REPRESENTATION_CONTEXT('','3D')
);
#11418=(
GEOMETRIC_REPRESENTATION_CONTEXT(3)
GLOBAL_UNCERTAINTY_ASSIGNED_CONTEXT((#11404))
GLOBAL_UNIT_ASSIGNED_CONTEXT((#11431,#11433,#11434))
REPRESENTATION_CONTEXT('','3D')
);
#11419=(
GEOMETRIC_REPRESENTATION_CONTEXT(3)
GLOBAL_UNCERTAINTY_ASSIGNED_CONTEXT((#11405))
GLOBAL_UNIT_ASSIGNED_CONTEXT((#11431,#11433,#11434))
REPRESENTATION_CONTEXT('','3D')
);
#11420=(
GEOMETRIC_REPRESENTATION_CONTEXT(3)
GLOBAL_UNCERTAINTY_ASSIGNED_CONTEXT((#11406))
GLOBAL_UNIT_ASSIGNED_CONTEXT((#11431,#11433,#11434))
REPRESENTATION_CONTEXT('','3D')
);
#11421=(
GEOMETRIC_REPRESENTATION_CONTEXT(3)
GLOBAL_UNCERTAINTY_ASSIGNED_CONTEXT((#11407))
GLOBAL_UNIT_ASSIGNED_CONTEXT((#11431,#11433,#11434))
REPRESENTATION_CONTEXT('','3D')
);
#11422=(
GEOMETRIC_REPRESENTATION_CONTEXT(3)
GLOBAL_UNCERTAINTY_ASSIGNED_CONTEXT((#11408))
GLOBAL_UNIT_ASSIGNED_CONTEXT((#11431,#11433,#11434))
REPRESENTATION_CONTEXT('','3D')
);
#11423=(
GEOMETRIC_REPRESENTATION_CONTEXT(3)
GLOBAL_UNCERTAINTY_ASSIGNED_CONTEXT((#11409))
GLOBAL_UNIT_ASSIGNED_CONTEXT((#11431,#11433,#11434))
REPRESENTATION_CONTEXT('','3D')
);
#11424=(
GEOMETRIC_REPRESENTATION_CONTEXT(3)
GLOBAL_UNCERTAINTY_ASSIGNED_CONTEXT((#11410))
GLOBAL_UNIT_ASSIGNED_CONTEXT((#11431,#11433,#11434))
REPRESENTATION_CONTEXT('','3D')
);
#11425=(
GEOMETRIC_REPRESENTATION_CONTEXT(3)
GLOBAL_UNCERTAINTY_ASSIGNED_CONTEXT((#11411))
GLOBAL_UNIT_ASSIGNED_CONTEXT((#11431,#11433,#11434))
REPRESENTATION_CONTEXT('','3D')
);
#11426=(
GEOMETRIC_REPRESENTATION_CONTEXT(3)
GLOBAL_UNCERTAINTY_ASSIGNED_CONTEXT((#11412))
GLOBAL_UNIT_ASSIGNED_CONTEXT((#11431,#11433,#11434))
REPRESENTATION_CONTEXT('','3D')
);
#11427=(
GEOMETRIC_REPRESENTATION_CONTEXT(3)
GLOBAL_UNCERTAINTY_ASSIGNED_CONTEXT((#11413))
GLOBAL_UNIT_ASSIGNED_CONTEXT((#11431,#11433,#11434))
REPRESENTATION_CONTEXT('','3D')
);
#11428=(
GEOMETRIC_REPRESENTATION_CONTEXT(3)
GLOBAL_UNCERTAINTY_ASSIGNED_CONTEXT((#11414))
GLOBAL_UNIT_ASSIGNED_CONTEXT((#11431,#11433,#11434))
REPRESENTATION_CONTEXT('','3D')
);
#11429=(
GEOMETRIC_REPRESENTATION_CONTEXT(3)
GLOBAL_UNCERTAINTY_ASSIGNED_CONTEXT((#11415))
GLOBAL_UNIT_ASSIGNED_CONTEXT((#11431,#11433,#11434))
REPRESENTATION_CONTEXT('','3D')
);
#11430=(
GEOMETRIC_REPRESENTATION_CONTEXT(3)
GLOBAL_UNCERTAINTY_ASSIGNED_CONTEXT((#11416))
GLOBAL_UNIT_ASSIGNED_CONTEXT((#11431,#11433,#11434))
REPRESENTATION_CONTEXT('','3D')
);
#11431=(
LENGTH_UNIT()
NAMED_UNIT(*)
SI_UNIT(.MILLI.,.METRE.)
);
#11432=(
LENGTH_UNIT()
NAMED_UNIT(*)
SI_UNIT($,.METRE.)
);
#11433=(
NAMED_UNIT(*)
PLANE_ANGLE_UNIT()
SI_UNIT($,.RADIAN.)
);
#11434=(
NAMED_UNIT(*)
SI_UNIT($,.STERADIAN.)
SOLID_ANGLE_UNIT()
);
#11435=SHAPE_DEFINITION_REPRESENTATION(#11448,#11478);
#11436=SHAPE_DEFINITION_REPRESENTATION(#11449,#11479);
#11437=SHAPE_DEFINITION_REPRESENTATION(#11450,#11480);
#11438=SHAPE_DEFINITION_REPRESENTATION(#11451,#11481);
#11439=SHAPE_DEFINITION_REPRESENTATION(#11452,#11482);
#11440=SHAPE_DEFINITION_REPRESENTATION(#11453,#11483);
#11441=SHAPE_DEFINITION_REPRESENTATION(#11454,#11484);
#11442=SHAPE_DEFINITION_REPRESENTATION(#11455,#11485);
#11443=SHAPE_DEFINITION_REPRESENTATION(#11456,#11486);
#11444=SHAPE_DEFINITION_REPRESENTATION(#11457,#11487);
#11445=SHAPE_DEFINITION_REPRESENTATION(#11458,#11488);
#11446=SHAPE_DEFINITION_REPRESENTATION(#11459,#11489);
#11447=SHAPE_DEFINITION_REPRESENTATION(#11460,#11490);
#11448=PRODUCT_DEFINITION_SHAPE('',$,#11492);
#11449=PRODUCT_DEFINITION_SHAPE('',$,#11493);
#11450=PRODUCT_DEFINITION_SHAPE('',$,#11494);
#11451=PRODUCT_DEFINITION_SHAPE('',$,#11495);
#11452=PRODUCT_DEFINITION_SHAPE('',$,#11496);
#11453=PRODUCT_DEFINITION_SHAPE('',$,#11497);
#11454=PRODUCT_DEFINITION_SHAPE('',$,#11498);
#11455=PRODUCT_DEFINITION_SHAPE('',$,#11499);
#11456=PRODUCT_DEFINITION_SHAPE('',$,#11500);
#11457=PRODUCT_DEFINITION_SHAPE('',$,#11501);
#11458=PRODUCT_DEFINITION_SHAPE('',$,#11502);
#11459=PRODUCT_DEFINITION_SHAPE('',$,#11503);
#11460=PRODUCT_DEFINITION_SHAPE('',$,#11504);
#11461=PRODUCT_DEFINITION_SHAPE($,$,#62);
#11462=PRODUCT_DEFINITION_SHAPE($,$,#63);
#11463=PRODUCT_DEFINITION_SHAPE($,$,#64);
#11464=PRODUCT_DEFINITION_SHAPE($,$,#65);
#11465=PRODUCT_DEFINITION_SHAPE($,$,#66);
#11466=PRODUCT_DEFINITION_SHAPE($,$,#67);
#11467=PRODUCT_DEFINITION_SHAPE($,$,#68);
#11468=PRODUCT_DEFINITION_SHAPE($,$,#69);
#11469=PRODUCT_DEFINITION_SHAPE($,$,#70);
#11470=PRODUCT_DEFINITION_SHAPE($,$,#71);
#11471=PRODUCT_DEFINITION_SHAPE($,$,#72);
#11472=PRODUCT_DEFINITION_SHAPE($,$,#73);
#11473=PRODUCT_DEFINITION_SHAPE($,$,#74);
#11474=PRODUCT_DEFINITION_SHAPE($,$,#75);
#11475=PRODUCT_DEFINITION_SHAPE($,$,#76);
#11476=PRODUCT_DEFINITION_SHAPE($,$,#77);
#11477=PRODUCT_DEFINITION_SHAPE($,$,#78);
#11478=SHAPE_REPRESENTATION('',(#4606,#5066,#5067,#5068,#5069,#5070,#5071,
#5072,#5073,#5074,#5075,#5076,#5077,#5078,#5079,#5080,#5081,#5082),#11417);
#11479=SHAPE_REPRESENTATION('',(#4607),#11418);
#11480=SHAPE_REPRESENTATION('',(#4677),#11419);
#11481=SHAPE_REPRESENTATION('',(#4700),#11420);
#11482=SHAPE_REPRESENTATION('',(#4733),#11421);
#11483=SHAPE_REPRESENTATION('',(#4742),#11422);
#11484=SHAPE_REPRESENTATION('',(#4806),#11423);
#11485=SHAPE_REPRESENTATION('',(#4843),#11424);
#11486=SHAPE_REPRESENTATION('',(#4897),#11425);
#11487=SHAPE_REPRESENTATION('',(#4914),#11426);
#11488=SHAPE_REPRESENTATION('',(#4977),#11427);
#11489=SHAPE_REPRESENTATION('',(#4990),#11428);
#11490=SHAPE_REPRESENTATION('',(#5047),#11429);
#11491=PRODUCT_DEFINITION_CONTEXT('part definition',#11532,'design');
#11492=PRODUCT_DEFINITION('2026-10-25-00-55-36-019','MAS-501',#11505,#11491);
#11493=PRODUCT_DEFINITION('2026-10-25-00-55-37-066',
'01_Pitch_Slider_Housing',#11506,#11491);
#11494=PRODUCT_DEFINITION('2026-10-25-00-55-37-452',
'02_Pitch_Slider_Sleeve_Brass',#11507,#11491);
#11495=PRODUCT_DEFINITION('2026-10-25-00-55-37-680',
'03_Ball_Bearing_MR106ZZ_6x10x3',#11508,#11491);
#11496=PRODUCT_DEFINITION('2026-10-25-00-55-37-835',
'04_Shim_Washer_6.1x8x0.5',#11509,#11491);
#11497=PRODUCT_DEFINITION('2026-10-25-00-55-37-930',
'05_Pitch_Yoke_Gold_Anodised',#11510,#11491);
#11498=PRODUCT_DEFINITION('2026-10-25-00-55-38-514',
'06_Set_Screw_ISO_4026_M2x2.5',#11511,#11491);
#11499=PRODUCT_DEFINITION('2026-10-25-00-55-40-821',
'11_Control_Ball_Stud_M2.5_D5.5',#11512,#11491);
#11500=PRODUCT_DEFINITION('2026-10-25-00-55-41-884',
'12_Tail_Output_Shaft_D5',#11513,#11491);
#11501=PRODUCT_DEFINITION('2026-10-25-00-55-38-878',
'07_Pitch_Link_Black',#11514,#11491);
#11502=PRODUCT_DEFINITION('2026-10-25-00-55-40-297',
'09_Pivot_Shoulder_Bushing',#11515,#11491);
#11503=PRODUCT_DEFINITION('2026-10-25-00-55-39-594',
'08_Pan_Head_Screw_ISO_7045_M2x5',#11516,#11491);
#11504=PRODUCT_DEFINITION('2026-10-25-00-55-40-595',
'10_Link_Bushing_D4x6.8',#11517,#11491);
#11505=PRODUCT_DEFINITION_FORMATION('',$,#11534);
#11506=PRODUCT_DEFINITION_FORMATION('',$,#11535);
#11507=PRODUCT_DEFINITION_FORMATION('',$,#11536);
#11508=PRODUCT_DEFINITION_FORMATION('',$,#11537);
#11509=PRODUCT_DEFINITION_FORMATION('',$,#11538);
#11510=PRODUCT_DEFINITION_FORMATION('',$,#11539);
#11511=PRODUCT_DEFINITION_FORMATION('',$,#11540);
#11512=PRODUCT_DEFINITION_FORMATION('',$,#11541);
#11513=PRODUCT_DEFINITION_FORMATION('',$,#11542);
#11514=PRODUCT_DEFINITION_FORMATION('',$,#11543);
#11515=PRODUCT_DEFINITION_FORMATION('',$,#11544);
#11516=PRODUCT_DEFINITION_FORMATION('',$,#11545);
#11517=PRODUCT_DEFINITION_FORMATION('',$,#11546);
#11518=PRODUCT_RELATED_PRODUCT_CATEGORY('MAS-501','MAS-501',(#11534));
#11519=PRODUCT_RELATED_PRODUCT_CATEGORY('01_Pitch_Slider_Housing',
'01_Pitch_Slider_Housing',(#11535));
#11520=PRODUCT_RELATED_PRODUCT_CATEGORY('02_Pitch_Slider_Sleeve_Brass',
'02_Pitch_Slider_Sleeve_Brass',(#11536));
#11521=PRODUCT_RELATED_PRODUCT_CATEGORY(
'03_Ball_Bearing_MR106ZZ_6x10x3','03_Ball_Bearing_MR106ZZ_6x10x3',(#11537));
#11522=PRODUCT_RELATED_PRODUCT_CATEGORY('04_Shim_Washer_6.1x8x0.5',
'04_Shim_Washer_6.1x8x0.5',(#11538));
#11523=PRODUCT_RELATED_PRODUCT_CATEGORY('05_Pitch_Yoke_Gold_Anodised',
'05_Pitch_Yoke_Gold_Anodised',(#11539));
#11524=PRODUCT_RELATED_PRODUCT_CATEGORY('06_Set_Screw_ISO_4026_M2x2.5',
'06_Set_Screw_ISO_4026_M2x2.5',(#11540));
#11525=PRODUCT_RELATED_PRODUCT_CATEGORY(
'11_Control_Ball_Stud_M2.5_D5.5','11_Control_Ball_Stud_M2.5_D5.5',(#11541));
#11526=PRODUCT_RELATED_PRODUCT_CATEGORY('12_Tail_Output_Shaft_D5',
'12_Tail_Output_Shaft_D5',(#11542));
#11527=PRODUCT_RELATED_PRODUCT_CATEGORY('07_Pitch_Link_Black',
'07_Pitch_Link_Black',(#11543));
#11528=PRODUCT_RELATED_PRODUCT_CATEGORY('09_Pivot_Shoulder_Bushing',
'09_Pivot_Shoulder_Bushing',(#11544));
#11529=PRODUCT_RELATED_PRODUCT_CATEGORY(
'08_Pan_Head_Screw_ISO_7045_M2x5','08_Pan_Head_Screw_ISO_7045_M2x5',(#11545));
#11530=PRODUCT_RELATED_PRODUCT_CATEGORY('10_Link_Bushing_D4x6.8',
'10_Link_Bushing_D4x6.8',(#11546));
#11531=APPLICATION_PROTOCOL_DEFINITION('international standard',
'automotive_design',2009,#11532);
#11532=APPLICATION_CONTEXT(
'Core Data for Automotive Mechanical Design Process');
#11533=PRODUCT_CONTEXT('part definition',#11532,'mechanical');
#11534=PRODUCT('2026-10-25-00-55-36-019','MAS-501',$,(#11533));
#11535=PRODUCT('2026-10-25-00-55-37-066','01_Pitch_Slider_Housing',$,(#11533));
#11536=PRODUCT('2026-10-25-00-55-37-452','02_Pitch_Slider_Sleeve_Brass',
$,(#11533));
#11537=PRODUCT('2026-10-25-00-55-37-680',
'03_Ball_Bearing_MR106ZZ_6x10x3',$,(#11533));
#11538=PRODUCT('2026-10-25-00-55-37-835','04_Shim_Washer_6.1x8x0.5',$,(#11533));
#11539=PRODUCT('2026-10-25-00-55-37-930','05_Pitch_Yoke_Gold_Anodised',
$,(#11533));
#11540=PRODUCT('2026-10-25-00-55-38-514','06_Set_Screw_ISO_4026_M2x2.5',
$,(#11533));
#11541=PRODUCT('2026-10-25-00-55-40-821',
'11_Control_Ball_Stud_M2.5_D5.5',$,(#11533));
#11542=PRODUCT('2026-10-25-00-55-41-884','12_Tail_Output_Shaft_D5',$,(#11533));
#11543=PRODUCT('2026-10-25-00-55-38-878','07_Pitch_Link_Black',$,(#11533));
#11544=PRODUCT('2026-10-25-00-55-40-297','09_Pivot_Shoulder_Bushing',$,
(#11533));
#11545=PRODUCT('2026-10-25-00-55-39-594',
'08_Pan_Head_Screw_ISO_7045_M2x5',$,(#11533));
#11546=PRODUCT('2026-10-25-00-55-40-595','10_Link_Bushing_D4x6.8',$,(#11533));
#11547=PRESENTATION_STYLE_ASSIGNMENT((#11552));
#11548=PRESENTATION_STYLE_ASSIGNMENT((#11553));
#11549=PRESENTATION_STYLE_ASSIGNMENT((#11554));
#11550=PRESENTATION_STYLE_ASSIGNMENT((#11555));
#11551=PRESENTATION_STYLE_ASSIGNMENT((#11556));
#11552=SURFACE_STYLE_USAGE(.BOTH.,#11557);
#11553=SURFACE_STYLE_USAGE(.BOTH.,#11558);
#11554=SURFACE_STYLE_USAGE(.BOTH.,#11559);
#11555=SURFACE_STYLE_USAGE(.BOTH.,#11560);
#11556=SURFACE_STYLE_USAGE(.BOTH.,#11561);
#11557=SURFACE_SIDE_STYLE('',(#11562));
#11558=SURFACE_SIDE_STYLE('',(#11563));
#11559=SURFACE_SIDE_STYLE('',(#11564));
#11560=SURFACE_SIDE_STYLE('',(#11565));
#11561=SURFACE_SIDE_STYLE('',(#11566));
#11562=SURFACE_STYLE_FILL_AREA(#11567);
#11563=SURFACE_STYLE_FILL_AREA(#11568);
#11564=SURFACE_STYLE_FILL_AREA(#11569);
#11565=SURFACE_STYLE_FILL_AREA(#11570);
#11566=SURFACE_STYLE_FILL_AREA(#11571);
#11567=FILL_AREA_STYLE('Steel - Satin',(#11572));
#11568=FILL_AREA_STYLE('MAS496_ss',(#11573));
#11569=FILL_AREA_STYLE('MAS496_ti',(#11574));
#11570=FILL_AREA_STYLE('MAS496_al',(#11575));
#11571=FILL_AREA_STYLE('MAS496_gun',(#11576));
#11572=FILL_AREA_STYLE_COLOUR('Steel - Satin',#11577);
#11573=FILL_AREA_STYLE_COLOUR('MAS496_ss',#11578);
#11574=FILL_AREA_STYLE_COLOUR('MAS496_ti',#11579);
#11575=FILL_AREA_STYLE_COLOUR('MAS496_al',#11580);
#11576=FILL_AREA_STYLE_COLOUR('MAS496_gun',#11581);
#11577=COLOUR_RGB('Steel - Satin',0.627450980392157,0.627450980392157,0.627450980392157);
#11578=COLOUR_RGB('MAS496_ss',0.83921568627451,0.850980392156863,0.862745098039216);
#11579=COLOUR_RGB('MAS496_ti',0.549019607843137,0.572549019607843,0.596078431372549);
#11580=COLOUR_RGB('MAS496_al',0.67843137254902,0.705882352941177,0.729411764705882);
#11581=COLOUR_RGB('MAS496_gun',0.313725490196078,0.337254901960784,0.364705882352941);
#11582=COLOUR_RGB('Dark Blue',0.08,0.2,0.34);
#11583=FILL_AREA_STYLE_COLOUR('',#11582);
#11584=FILL_AREA_STYLE('',(#11583));
#11585=SURFACE_STYLE_FILL_AREA(#11584);
#11586=SURFACE_SIDE_STYLE('',(#11585));
#11587=SURFACE_STYLE_USAGE(.BOTH.,#11586);
#11588=PRESENTATION_STYLE_ASSIGNMENT((#11587));
#11589=COLOUR_RGB('Light Blue',0.38,0.62,0.78);
#11590=FILL_AREA_STYLE_COLOUR('',#11589);
#11591=FILL_AREA_STYLE('',(#11590));
#11592=SURFACE_STYLE_FILL_AREA(#11591);
#11593=SURFACE_SIDE_STYLE('',(#11592));
#11594=SURFACE_STYLE_USAGE(.BOTH.,#11593);
#11595=PRESENTATION_STYLE_ASSIGNMENT((#11594));
#11596=COLOUR_RGB('Sky Blue',0.24,0.69,0.87);
#11597=FILL_AREA_STYLE_COLOUR('',#11596);
#11598=FILL_AREA_STYLE('',(#11597));
#11599=SURFACE_STYLE_FILL_AREA(#11598);
#11600=SURFACE_SIDE_STYLE('',(#11599));
#11601=SURFACE_STYLE_USAGE(.BOTH.,#11600);
#11602=PRESENTATION_STYLE_ASSIGNMENT((#11601));
#11603=COLOUR_RGB('Grey',0.48,0.52,0.57);
#11604=FILL_AREA_STYLE_COLOUR('',#11603);
#11605=FILL_AREA_STYLE('',(#11604));
#11606=SURFACE_STYLE_FILL_AREA(#11605);
#11607=SURFACE_SIDE_STYLE('',(#11606));
#11608=SURFACE_STYLE_USAGE(.BOTH.,#11607);
#11609=PRESENTATION_STYLE_ASSIGNMENT((#11608));
#11610=COLOUR_RGB('Black',0.12,0.14,0.17);
#11611=FILL_AREA_STYLE_COLOUR('',#11610);
#11612=FILL_AREA_STYLE('',(#11611));
#11613=SURFACE_STYLE_FILL_AREA(#11612);
#11614=SURFACE_SIDE_STYLE('',(#11613));
#11615=SURFACE_STYLE_USAGE(.BOTH.,#11614);
#11616=PRESENTATION_STYLE_ASSIGNMENT((#11615));
#11617=COLOUR_RGB('Off White',0.89,0.88,0.83);
#11618=FILL_AREA_STYLE_COLOUR('',#11617);
#11619=FILL_AREA_STYLE('',(#11618));
#11620=SURFACE_STYLE_FILL_AREA(#11619);
#11621=SURFACE_SIDE_STYLE('',(#11620));
#11622=SURFACE_STYLE_USAGE(.BOTH.,#11621);
#11623=PRESENTATION_STYLE_ASSIGNMENT((#11622));
ENDSEC;
END-ISO-10303-21;
